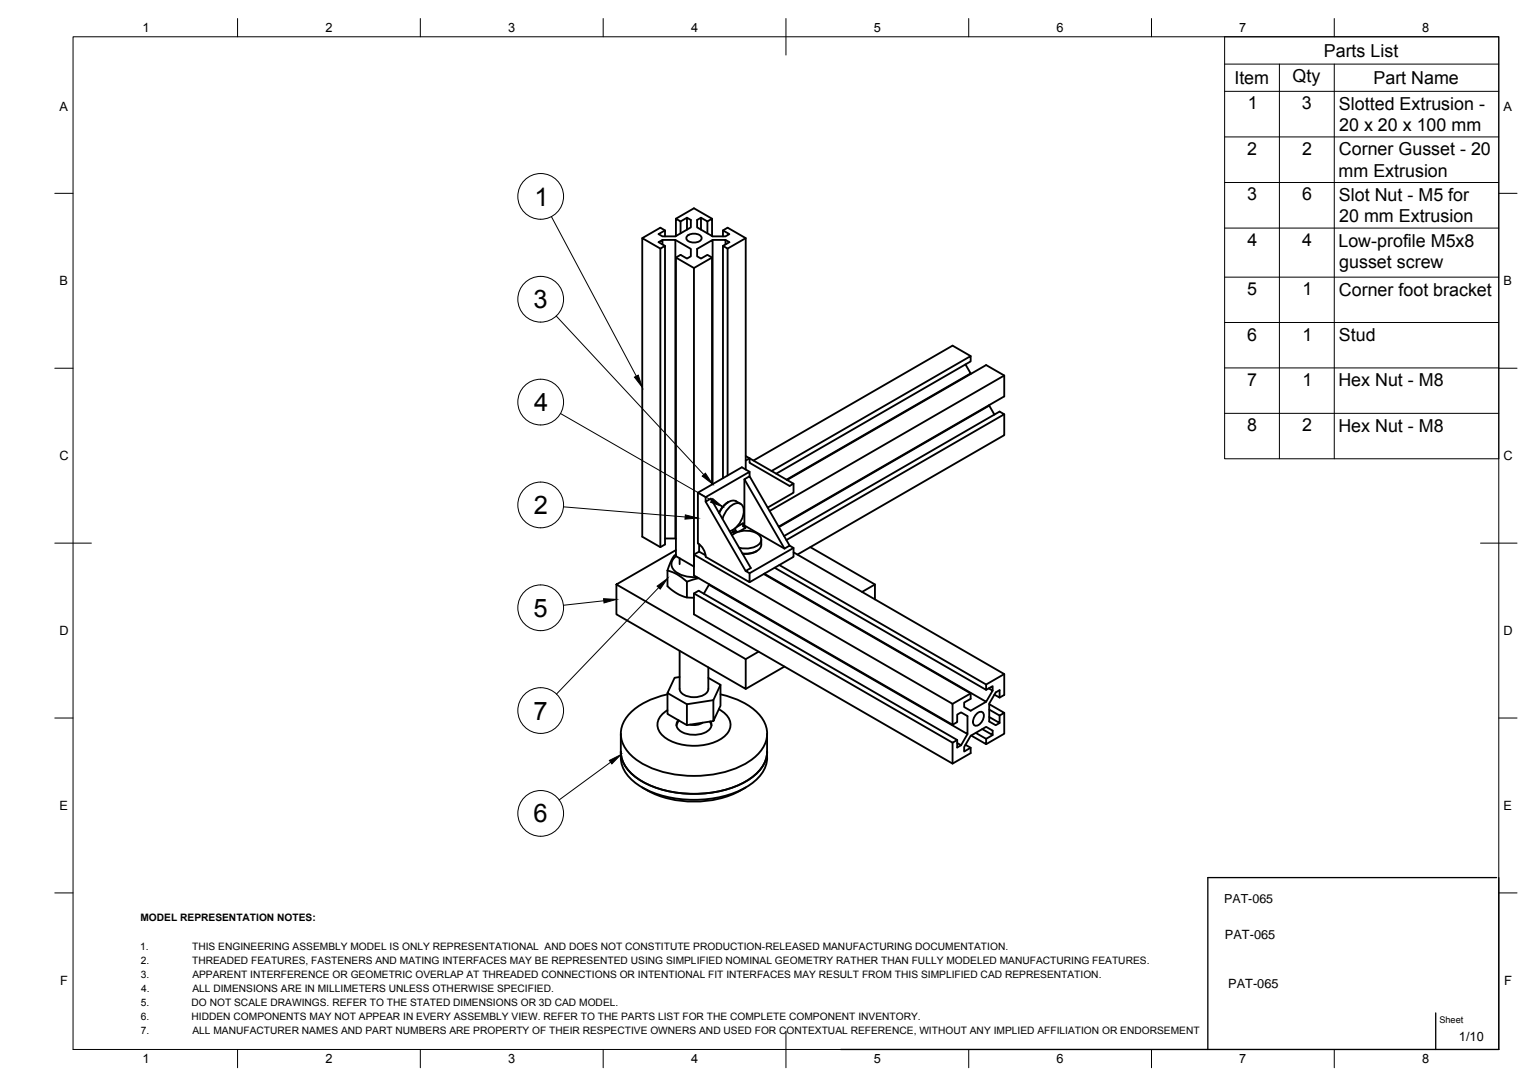
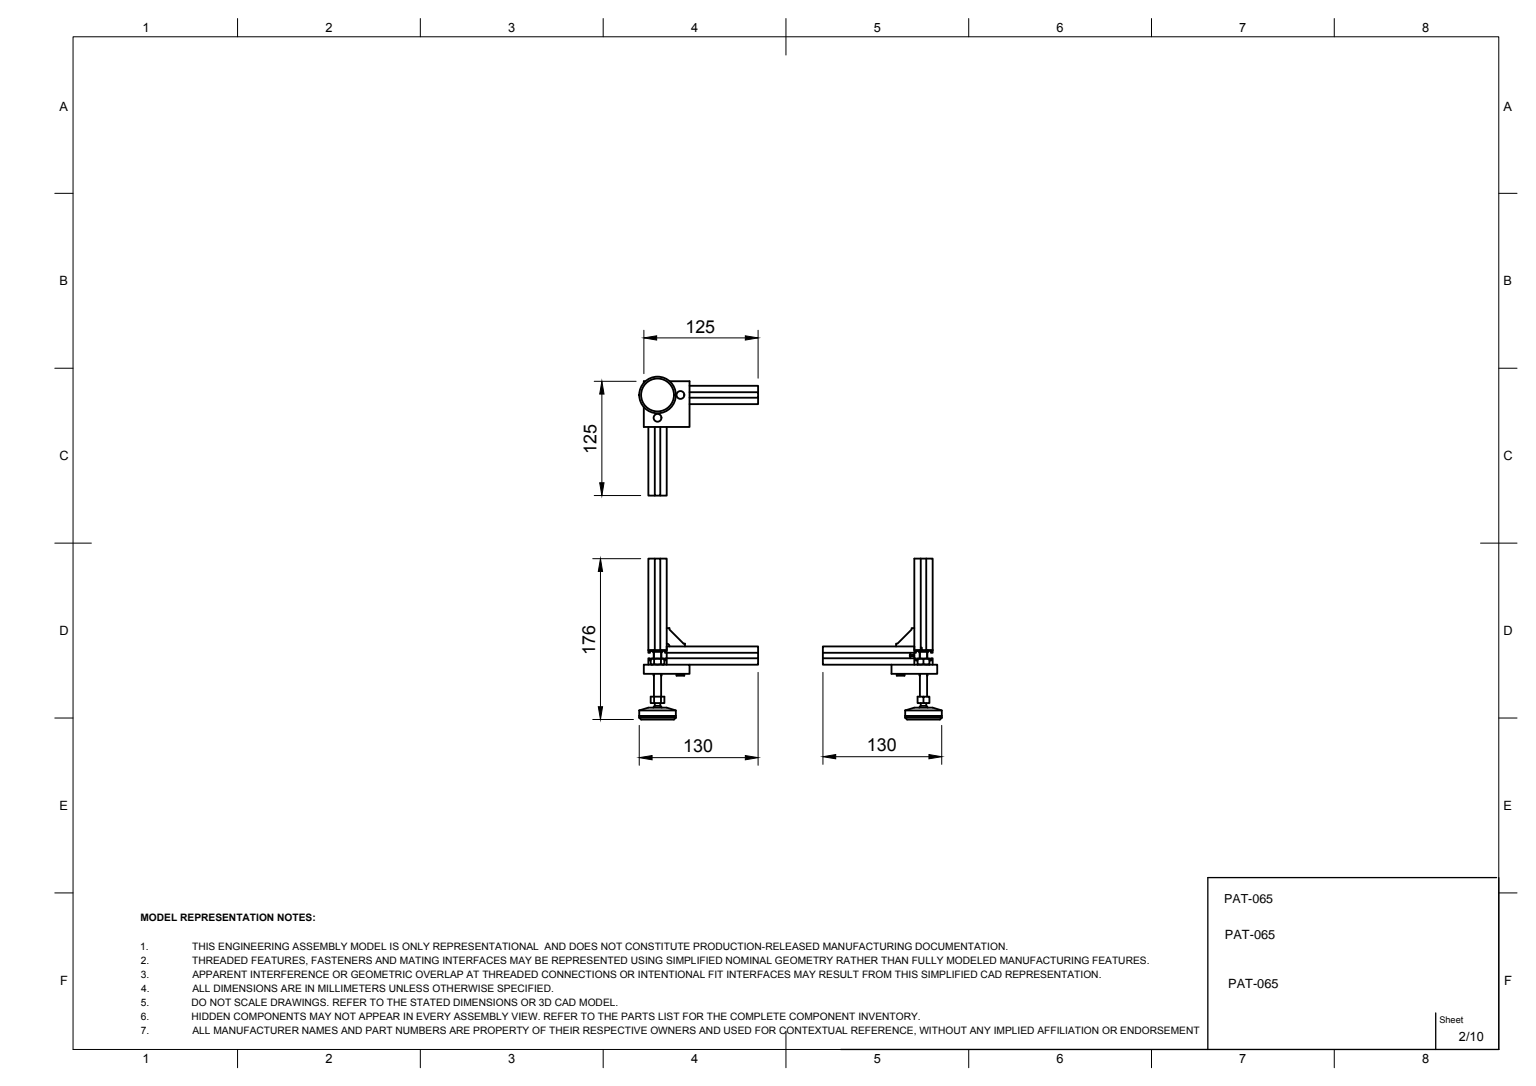
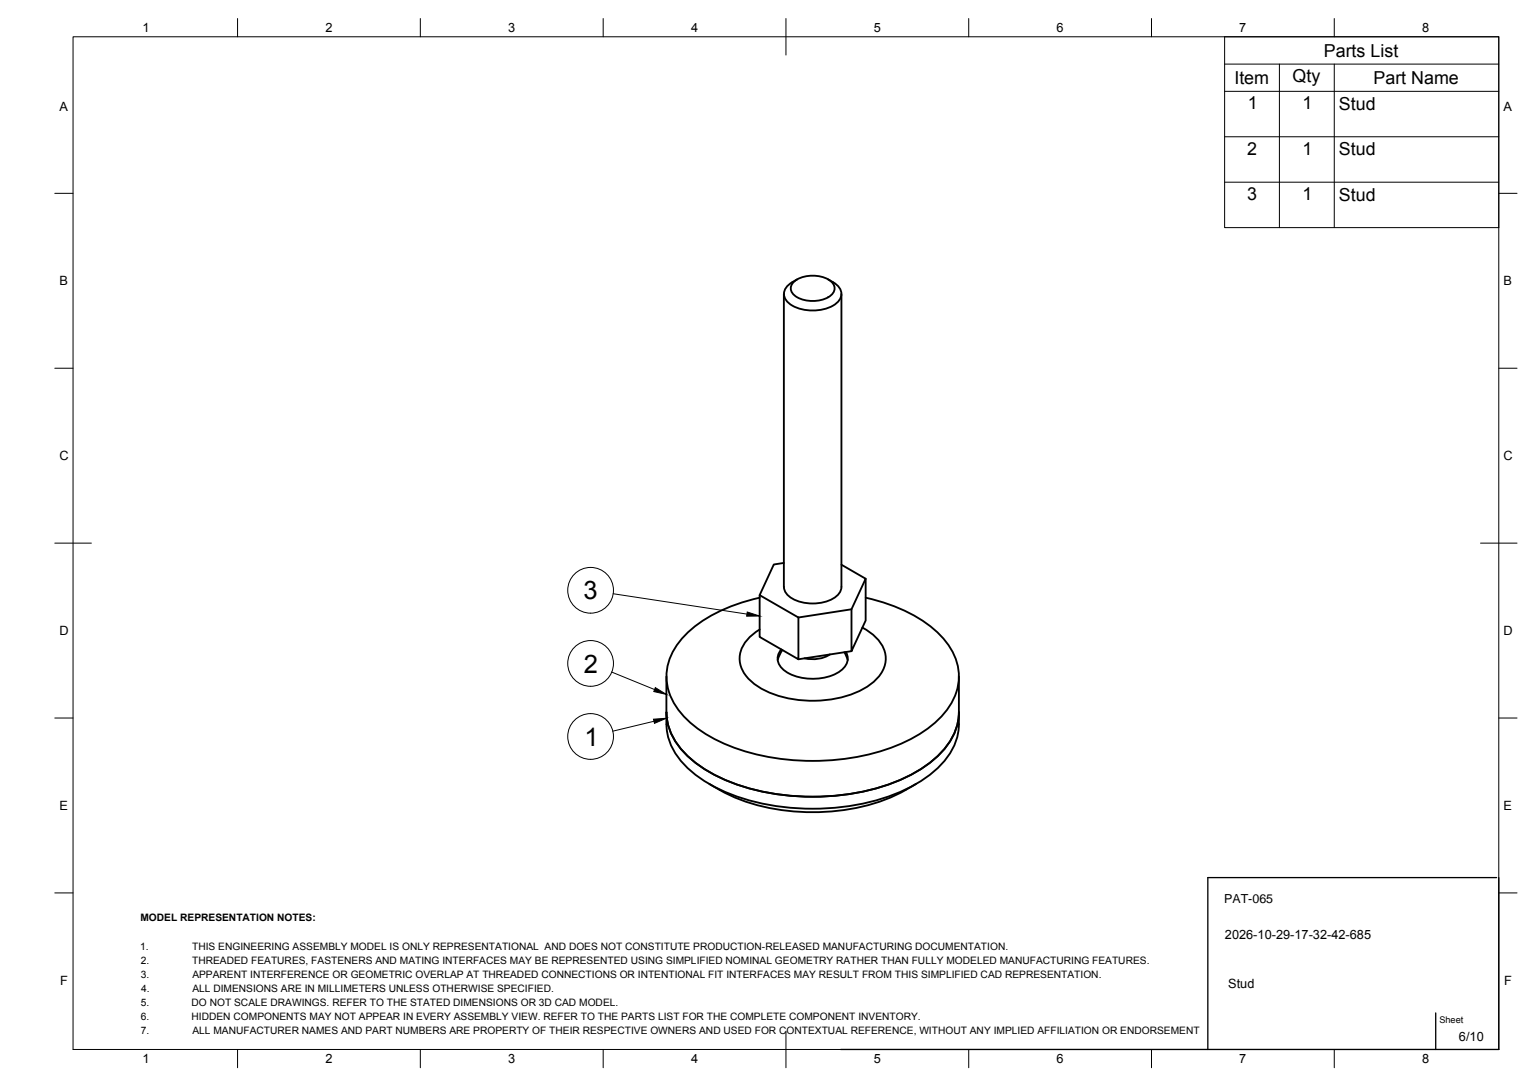
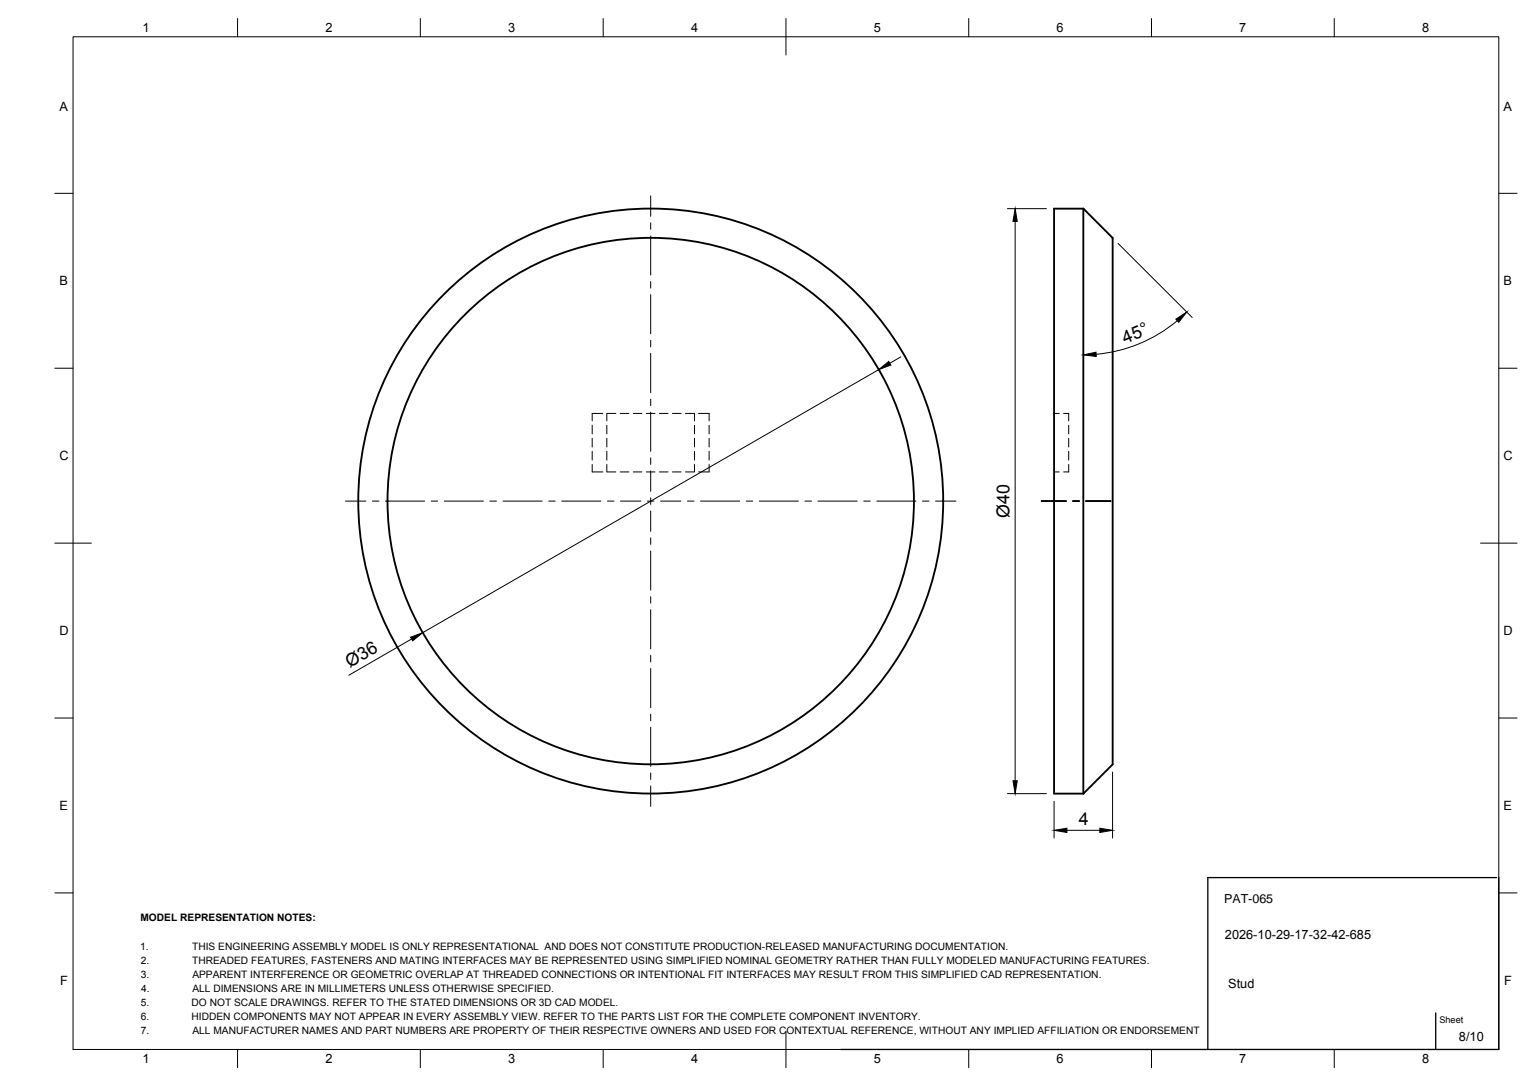
ISO-10303-21;
HEADER;
/* Generated by software containing ST-Developer
 * from STEP Tools, Inc. (www.steptools.com) 
 */

FILE_DESCRIPTION(
/* description */ ('PAT-065'),
/* implementation_level */ '2;1');

FILE_NAME(
/* name */ 'PAT-065',
/* time_stamp */ '2026-10-28T22:09:22-07:00',
/* author */ (''),
/* organization */ (''),
/* preprocessor_version */ 'ST-DEVELOPER v20.2',
/* originating_system */ 'Autodesk Translation Framework v15.17.0.0',
/* authorisation */ '');

FILE_SCHEMA (('AUTOMOTIVE_DESIGN { 1 0 10303 214 3 1 1 }'));
ENDSEC;

DATA;
#10=MECHANICAL_DESIGN_GEOMETRIC_PRESENTATION_REPRESENTATION('',(#158,#159,
#160,#161,#162,#163,#164,#165,#166,#167),#5502);
#11=(
BOUNDED_CURVE()
B_SPLINE_CURVE(2,(#5238,#5239,#5240),.UNSPECIFIED.,.F.,.F.)
B_SPLINE_CURVE_WITH_KNOTS((3,3),(0.14973948338295,0.97160236658079),
 .UNSPECIFIED.)
CURVE()
GEOMETRIC_REPRESENTATION_ITEM()
RATIONAL_B_SPLINE_CURVE((1.07140024848292,1.23714644374248,1.07140024848292))
REPRESENTATION_ITEM('')
);
#12=(
BOUNDED_CURVE()
B_SPLINE_CURVE(2,(#5242,#5243,#5244),.UNSPECIFIED.,.F.,.F.)
B_SPLINE_CURVE_WITH_KNOTS((3,3),(0.14973948338295,0.971602366580789),
 .UNSPECIFIED.)
CURVE()
GEOMETRIC_REPRESENTATION_ITEM()
RATIONAL_B_SPLINE_CURVE((1.07140024848292,1.23714644374248,1.07140024848292))
REPRESENTATION_ITEM('')
);
#13=(
BOUNDED_CURVE()
B_SPLINE_CURVE(2,(#5249,#5250,#5251),.UNSPECIFIED.,.F.,.F.)
B_SPLINE_CURVE_WITH_KNOTS((3,3),(0.14973948338295,0.97160236658079),
 .UNSPECIFIED.)
CURVE()
GEOMETRIC_REPRESENTATION_ITEM()
RATIONAL_B_SPLINE_CURVE((1.07140024848292,1.23714644374248,1.07140024848292))
REPRESENTATION_ITEM('')
);
#14=(
BOUNDED_CURVE()
B_SPLINE_CURVE(2,(#5253,#5254,#5255),.UNSPECIFIED.,.F.,.F.)
B_SPLINE_CURVE_WITH_KNOTS((3,3),(0.14973948338295,0.97160236658079),
 .UNSPECIFIED.)
CURVE()
GEOMETRIC_REPRESENTATION_ITEM()
RATIONAL_B_SPLINE_CURVE((1.07140024848292,1.23714644374248,1.07140024848292))
REPRESENTATION_ITEM('')
);
#15=(
BOUNDED_CURVE()
B_SPLINE_CURVE(2,(#5257,#5258,#5259),.UNSPECIFIED.,.F.,.F.)
B_SPLINE_CURVE_WITH_KNOTS((3,3),(0.14973948338295,0.971602366580789),
 .UNSPECIFIED.)
CURVE()
GEOMETRIC_REPRESENTATION_ITEM()
RATIONAL_B_SPLINE_CURVE((1.07140024848292,1.23714644374248,1.07140024848292))
REPRESENTATION_ITEM('')
);
#16=(
BOUNDED_CURVE()
B_SPLINE_CURVE(2,(#5260,#5261,#5262),.UNSPECIFIED.,.F.,.F.)
B_SPLINE_CURVE_WITH_KNOTS((3,3),(0.14973948338295,0.97160236658079),
 .UNSPECIFIED.)
CURVE()
GEOMETRIC_REPRESENTATION_ITEM()
RATIONAL_B_SPLINE_CURVE((1.07140024848292,1.23714644374248,1.07140024848292))
REPRESENTATION_ITEM('')
);
#17=(
BOUNDED_CURVE()
B_SPLINE_CURVE(2,(#5269,#5270,#5271),.UNSPECIFIED.,.F.,.F.)
B_SPLINE_CURVE_WITH_KNOTS((3,3),(0.14973948338295,0.97160236658079),
 .UNSPECIFIED.)
CURVE()
GEOMETRIC_REPRESENTATION_ITEM()
RATIONAL_B_SPLINE_CURVE((1.07140024848292,1.23714644374248,1.07140024848292))
REPRESENTATION_ITEM('')
);
#18=(
BOUNDED_CURVE()
B_SPLINE_CURVE(2,(#5273,#5274,#5275),.UNSPECIFIED.,.F.,.F.)
B_SPLINE_CURVE_WITH_KNOTS((3,3),(0.14973948338295,0.97160236658079),
 .UNSPECIFIED.)
CURVE()
GEOMETRIC_REPRESENTATION_ITEM()
RATIONAL_B_SPLINE_CURVE((1.07140024848292,1.23714644374248,1.07140024848292))
REPRESENTATION_ITEM('')
);
#19=(
BOUNDED_CURVE()
B_SPLINE_CURVE(2,(#5277,#5278,#5279),.UNSPECIFIED.,.F.,.F.)
B_SPLINE_CURVE_WITH_KNOTS((3,3),(0.14973948338295,0.971602366580789),
 .UNSPECIFIED.)
CURVE()
GEOMETRIC_REPRESENTATION_ITEM()
RATIONAL_B_SPLINE_CURVE((1.07140024848292,1.23714644374248,1.07140024848292))
REPRESENTATION_ITEM('')
);
#20=(
BOUNDED_CURVE()
B_SPLINE_CURVE(2,(#5281,#5282,#5283),.UNSPECIFIED.,.F.,.F.)
B_SPLINE_CURVE_WITH_KNOTS((3,3),(0.14973948338295,0.97160236658079),
 .UNSPECIFIED.)
CURVE()
GEOMETRIC_REPRESENTATION_ITEM()
RATIONAL_B_SPLINE_CURVE((1.07140024848292,1.23714644374248,1.07140024848292))
REPRESENTATION_ITEM('')
);
#21=(
BOUNDED_CURVE()
B_SPLINE_CURVE(2,(#5285,#5286,#5287),.UNSPECIFIED.,.F.,.F.)
B_SPLINE_CURVE_WITH_KNOTS((3,3),(0.14973948338295,0.97160236658079),
 .UNSPECIFIED.)
CURVE()
GEOMETRIC_REPRESENTATION_ITEM()
RATIONAL_B_SPLINE_CURVE((1.07140024848292,1.23714644374248,1.07140024848292))
REPRESENTATION_ITEM('')
);
#22=(
BOUNDED_CURVE()
B_SPLINE_CURVE(2,(#5288,#5289,#5290),.UNSPECIFIED.,.F.,.F.)
B_SPLINE_CURVE_WITH_KNOTS((3,3),(0.14973948338295,0.971602366580789),
 .UNSPECIFIED.)
CURVE()
GEOMETRIC_REPRESENTATION_ITEM()
RATIONAL_B_SPLINE_CURVE((1.07140024848292,1.23714644374248,1.07140024848292))
REPRESENTATION_ITEM('')
);
#23=ITEM_DEFINED_TRANSFORMATION($,$,#3464,#3521);
#24=ITEM_DEFINED_TRANSFORMATION($,$,#3481,#3522);
#25=ITEM_DEFINED_TRANSFORMATION($,$,#3496,#3523);
#26=ITEM_DEFINED_TRANSFORMATION($,$,#3328,#3598);
#27=ITEM_DEFINED_TRANSFORMATION($,$,#3344,#3599);
#28=ITEM_DEFINED_TRANSFORMATION($,$,#3344,#3600);
#29=ITEM_DEFINED_TRANSFORMATION($,$,#3344,#3601);
#30=ITEM_DEFINED_TRANSFORMATION($,$,#3411,#3602);
#31=ITEM_DEFINED_TRANSFORMATION($,$,#3411,#3603);
#32=ITEM_DEFINED_TRANSFORMATION($,$,#3548,#3604);
#33=ITEM_DEFINED_TRANSFORMATION($,$,#3442,#3605);
#34=ITEM_DEFINED_TRANSFORMATION($,$,#3548,#3606);
#35=ITEM_DEFINED_TRANSFORMATION($,$,#3442,#3607);
#36=ITEM_DEFINED_TRANSFORMATION($,$,#3548,#3608);
#37=ITEM_DEFINED_TRANSFORMATION($,$,#3442,#3609);
#38=ITEM_DEFINED_TRANSFORMATION($,$,#3548,#3610);
#39=ITEM_DEFINED_TRANSFORMATION($,$,#3442,#3611);
#40=ITEM_DEFINED_TRANSFORMATION($,$,#3463,#3612);
#41=ITEM_DEFINED_TRANSFORMATION($,$,#3524,#3613);
#42=ITEM_DEFINED_TRANSFORMATION($,$,#3548,#3614);
#43=ITEM_DEFINED_TRANSFORMATION($,$,#3577,#3615);
#44=ITEM_DEFINED_TRANSFORMATION($,$,#3548,#3616);
#45=ITEM_DEFINED_TRANSFORMATION($,$,#3577,#3617);
#46=(
REPRESENTATION_RELATIONSHIP($,$,#5560,#5559)
REPRESENTATION_RELATIONSHIP_WITH_TRANSFORMATION(#23)
SHAPE_REPRESENTATION_RELATIONSHIP()
);
#47=(
REPRESENTATION_RELATIONSHIP($,$,#5561,#5559)
REPRESENTATION_RELATIONSHIP_WITH_TRANSFORMATION(#24)
SHAPE_REPRESENTATION_RELATIONSHIP()
);
#48=(
REPRESENTATION_RELATIONSHIP($,$,#5562,#5559)
REPRESENTATION_RELATIONSHIP_WITH_TRANSFORMATION(#25)
SHAPE_REPRESENTATION_RELATIONSHIP()
);
#49=(
REPRESENTATION_RELATIONSHIP($,$,#5555,#5554)
REPRESENTATION_RELATIONSHIP_WITH_TRANSFORMATION(#26)
SHAPE_REPRESENTATION_RELATIONSHIP()
);
#50=(
REPRESENTATION_RELATIONSHIP($,$,#5556,#5554)
REPRESENTATION_RELATIONSHIP_WITH_TRANSFORMATION(#27)
SHAPE_REPRESENTATION_RELATIONSHIP()
);
#51=(
REPRESENTATION_RELATIONSHIP($,$,#5556,#5554)
REPRESENTATION_RELATIONSHIP_WITH_TRANSFORMATION(#28)
SHAPE_REPRESENTATION_RELATIONSHIP()
);
#52=(
REPRESENTATION_RELATIONSHIP($,$,#5556,#5554)
REPRESENTATION_RELATIONSHIP_WITH_TRANSFORMATION(#29)
SHAPE_REPRESENTATION_RELATIONSHIP()
);
#53=(
REPRESENTATION_RELATIONSHIP($,$,#5557,#5554)
REPRESENTATION_RELATIONSHIP_WITH_TRANSFORMATION(#30)
SHAPE_REPRESENTATION_RELATIONSHIP()
);
#54=(
REPRESENTATION_RELATIONSHIP($,$,#5557,#5554)
REPRESENTATION_RELATIONSHIP_WITH_TRANSFORMATION(#31)
SHAPE_REPRESENTATION_RELATIONSHIP()
);
#55=(
REPRESENTATION_RELATIONSHIP($,$,#5564,#5554)
REPRESENTATION_RELATIONSHIP_WITH_TRANSFORMATION(#32)
SHAPE_REPRESENTATION_RELATIONSHIP()
);
#56=(
REPRESENTATION_RELATIONSHIP($,$,#5558,#5554)
REPRESENTATION_RELATIONSHIP_WITH_TRANSFORMATION(#33)
SHAPE_REPRESENTATION_RELATIONSHIP()
);
#57=(
REPRESENTATION_RELATIONSHIP($,$,#5564,#5554)
REPRESENTATION_RELATIONSHIP_WITH_TRANSFORMATION(#34)
SHAPE_REPRESENTATION_RELATIONSHIP()
);
#58=(
REPRESENTATION_RELATIONSHIP($,$,#5558,#5554)
REPRESENTATION_RELATIONSHIP_WITH_TRANSFORMATION(#35)
SHAPE_REPRESENTATION_RELATIONSHIP()
);
#59=(
REPRESENTATION_RELATIONSHIP($,$,#5564,#5554)
REPRESENTATION_RELATIONSHIP_WITH_TRANSFORMATION(#36)
SHAPE_REPRESENTATION_RELATIONSHIP()
);
#60=(
REPRESENTATION_RELATIONSHIP($,$,#5558,#5554)
REPRESENTATION_RELATIONSHIP_WITH_TRANSFORMATION(#37)
SHAPE_REPRESENTATION_RELATIONSHIP()
);
#61=(
REPRESENTATION_RELATIONSHIP($,$,#5564,#5554)
REPRESENTATION_RELATIONSHIP_WITH_TRANSFORMATION(#38)
SHAPE_REPRESENTATION_RELATIONSHIP()
);
#62=(
REPRESENTATION_RELATIONSHIP($,$,#5558,#5554)
REPRESENTATION_RELATIONSHIP_WITH_TRANSFORMATION(#39)
SHAPE_REPRESENTATION_RELATIONSHIP()
);
#63=(
REPRESENTATION_RELATIONSHIP($,$,#5559,#5554)
REPRESENTATION_RELATIONSHIP_WITH_TRANSFORMATION(#40)
SHAPE_REPRESENTATION_RELATIONSHIP()
);
#64=(
REPRESENTATION_RELATIONSHIP($,$,#5563,#5554)
REPRESENTATION_RELATIONSHIP_WITH_TRANSFORMATION(#41)
SHAPE_REPRESENTATION_RELATIONSHIP()
);
#65=(
REPRESENTATION_RELATIONSHIP($,$,#5564,#5554)
REPRESENTATION_RELATIONSHIP_WITH_TRANSFORMATION(#42)
SHAPE_REPRESENTATION_RELATIONSHIP()
);
#66=(
REPRESENTATION_RELATIONSHIP($,$,#5565,#5554)
REPRESENTATION_RELATIONSHIP_WITH_TRANSFORMATION(#43)
SHAPE_REPRESENTATION_RELATIONSHIP()
);
#67=(
REPRESENTATION_RELATIONSHIP($,$,#5564,#5554)
REPRESENTATION_RELATIONSHIP_WITH_TRANSFORMATION(#44)
SHAPE_REPRESENTATION_RELATIONSHIP()
);
#68=(
REPRESENTATION_RELATIONSHIP($,$,#5565,#5554)
REPRESENTATION_RELATIONSHIP_WITH_TRANSFORMATION(#45)
SHAPE_REPRESENTATION_RELATIONSHIP()
);
#69=CONTEXT_DEPENDENT_SHAPE_REPRESENTATION(#46,#5528);
#70=CONTEXT_DEPENDENT_SHAPE_REPRESENTATION(#47,#5529);
#71=CONTEXT_DEPENDENT_SHAPE_REPRESENTATION(#48,#5530);
#72=CONTEXT_DEPENDENT_SHAPE_REPRESENTATION(#49,#5534);
#73=CONTEXT_DEPENDENT_SHAPE_REPRESENTATION(#50,#5535);
#74=CONTEXT_DEPENDENT_SHAPE_REPRESENTATION(#51,#5536);
#75=CONTEXT_DEPENDENT_SHAPE_REPRESENTATION(#52,#5537);
#76=CONTEXT_DEPENDENT_SHAPE_REPRESENTATION(#53,#5538);
#77=CONTEXT_DEPENDENT_SHAPE_REPRESENTATION(#54,#5539);
#78=CONTEXT_DEPENDENT_SHAPE_REPRESENTATION(#55,#5540);
#79=CONTEXT_DEPENDENT_SHAPE_REPRESENTATION(#56,#5541);
#80=CONTEXT_DEPENDENT_SHAPE_REPRESENTATION(#57,#5542);
#81=CONTEXT_DEPENDENT_SHAPE_REPRESENTATION(#58,#5543);
#82=CONTEXT_DEPENDENT_SHAPE_REPRESENTATION(#59,#5544);
#83=CONTEXT_DEPENDENT_SHAPE_REPRESENTATION(#60,#5545);
#84=CONTEXT_DEPENDENT_SHAPE_REPRESENTATION(#61,#5546);
#85=CONTEXT_DEPENDENT_SHAPE_REPRESENTATION(#62,#5547);
#86=CONTEXT_DEPENDENT_SHAPE_REPRESENTATION(#63,#5548);
#87=CONTEXT_DEPENDENT_SHAPE_REPRESENTATION(#64,#5549);
#88=CONTEXT_DEPENDENT_SHAPE_REPRESENTATION(#65,#5550);
#89=CONTEXT_DEPENDENT_SHAPE_REPRESENTATION(#66,#5551);
#90=CONTEXT_DEPENDENT_SHAPE_REPRESENTATION(#67,#5552);
#91=CONTEXT_DEPENDENT_SHAPE_REPRESENTATION(#68,#5553);
#92=NEXT_ASSEMBLY_USAGE_OCCURRENCE('Rubber base:1','Rubber base:1',
'Rubber base:1',#5572,#5573,'Rubber base:1');
#93=NEXT_ASSEMBLY_USAGE_OCCURRENCE('Steel pad:1','Steel pad:1',
'Steel pad:1',#5572,#5574,'Steel pad:1');
#94=NEXT_ASSEMBLY_USAGE_OCCURRENCE('Stud:1','Stud:1','Stud:1',#5572,#5575,
'Stud:1');
#95=NEXT_ASSEMBLY_USAGE_OCCURRENCE('Corner foot bracket:1',
'Corner foot bracket:1','Corner foot bracket:1',#5567,#5568,
'Corner foot bracket:1');
#96=NEXT_ASSEMBLY_USAGE_OCCURRENCE(
'Slotted Extrusion - 20 x 20 x 100 mm:1',
'Slotted Extrusion - 20 x 20 x 100 mm:1',
'Slotted Extrusion - 20 x 20 x 100 mm:1',#5567,#5569,
'Slotted Extrusion - 20 x 20 x 100 mm:1');
#97=NEXT_ASSEMBLY_USAGE_OCCURRENCE(
'Slotted Extrusion - 20 x 20 x 100 mm:2',
'Slotted Extrusion - 20 x 20 x 100 mm:2',
'Slotted Extrusion - 20 x 20 x 100 mm:2',#5567,#5569,
'Slotted Extrusion - 20 x 20 x 100 mm:2');
#98=NEXT_ASSEMBLY_USAGE_OCCURRENCE(
'Slotted Extrusion - 20 x 20 x 100 mm:3',
'Slotted Extrusion - 20 x 20 x 100 mm:3',
'Slotted Extrusion - 20 x 20 x 100 mm:3',#5567,#5569,
'Slotted Extrusion - 20 x 20 x 100 mm:3');
#99=NEXT_ASSEMBLY_USAGE_OCCURRENCE('Corner Gusset - 20 mm Extrusion:1',
'Corner Gusset - 20 mm Extrusion:1','Corner Gusset - 20 mm Extrusion:1',
#5567,#5570,'Corner Gusset - 20 mm Extrusion:1');
#100=NEXT_ASSEMBLY_USAGE_OCCURRENCE('Corner Gusset - 20 mm Extrusion:2',
'Corner Gusset - 20 mm Extrusion:2','Corner Gusset - 20 mm Extrusion:2',
#5567,#5570,'Corner Gusset - 20 mm Extrusion:2');
#101=NEXT_ASSEMBLY_USAGE_OCCURRENCE(
'Slot Nut - M5 for 20 mm Extrusion:1',
'Slot Nut - M5 for 20 mm Extrusion:1',
'Slot Nut - M5 for 20 mm Extrusion:1',#5567,#5577,
'Slot Nut - M5 for 20 mm Extrusion:1');
#102=NEXT_ASSEMBLY_USAGE_OCCURRENCE('Low-profile M5x8 gusset screw:1',
'Low-profile M5x8 gusset screw:1','Low-profile M5x8 gusset screw:1',#5567,
#5571,'Low-profile M5x8 gusset screw:1');
#103=NEXT_ASSEMBLY_USAGE_OCCURRENCE(
'Slot Nut - M5 for 20 mm Extrusion:2',
'Slot Nut - M5 for 20 mm Extrusion:2',
'Slot Nut - M5 for 20 mm Extrusion:2',#5567,#5577,
'Slot Nut - M5 for 20 mm Extrusion:2');
#104=NEXT_ASSEMBLY_USAGE_OCCURRENCE('Low-profile M5x8 gusset screw:2',
'Low-profile M5x8 gusset screw:2','Low-profile M5x8 gusset screw:2',#5567,
#5571,'Low-profile M5x8 gusset screw:2');
#105=NEXT_ASSEMBLY_USAGE_OCCURRENCE(
'Slot Nut - M5 for 20 mm Extrusion:3',
'Slot Nut - M5 for 20 mm Extrusion:3',
'Slot Nut - M5 for 20 mm Extrusion:3',#5567,#5577,
'Slot Nut - M5 for 20 mm Extrusion:3');
#106=NEXT_ASSEMBLY_USAGE_OCCURRENCE('Low-profile M5x8 gusset screw:3',
'Low-profile M5x8 gusset screw:3','Low-profile M5x8 gusset screw:3',#5567,
#5571,'Low-profile M5x8 gusset screw:3');
#107=NEXT_ASSEMBLY_USAGE_OCCURRENCE(
'Slot Nut - M5 for 20 mm Extrusion:4',
'Slot Nut - M5 for 20 mm Extrusion:4',
'Slot Nut - M5 for 20 mm Extrusion:4',#5567,#5577,
'Slot Nut - M5 for 20 mm Extrusion:4');
#108=NEXT_ASSEMBLY_USAGE_OCCURRENCE('Low-profile M5x8 gusset screw:4',
'Low-profile M5x8 gusset screw:4','Low-profile M5x8 gusset screw:4',#5567,
#5571,'Low-profile M5x8 gusset screw:4');
#109=NEXT_ASSEMBLY_USAGE_OCCURRENCE(
'Levelling Foot - 40 mm Pad, M8 Stud:1',
'Levelling Foot - 40 mm Pad, M8 Stud:1',
'Levelling Foot - 40 mm Pad, M8 Stud:1',#5567,#5572,
'Levelling Foot - 40 mm Pad, M8 Stud:1');
#110=NEXT_ASSEMBLY_USAGE_OCCURRENCE('Hex Nut - M8:1','Hex Nut - M8:1',
'Hex Nut - M8:1',#5567,#5576,'Hex Nut - M8:1');
#111=NEXT_ASSEMBLY_USAGE_OCCURRENCE(
'Slot Nut - M5 for 20 mm Extrusion:5',
'Slot Nut - M5 for 20 mm Extrusion:5',
'Slot Nut - M5 for 20 mm Extrusion:5',#5567,#5577,
'Slot Nut - M5 for 20 mm Extrusion:5');
#112=NEXT_ASSEMBLY_USAGE_OCCURRENCE('M5x14 Cap Screw:1',
'M5x14 Cap Screw:1','M5x14 Cap Screw:1',#5567,#5578,'M5x14 Cap Screw:1');
#113=NEXT_ASSEMBLY_USAGE_OCCURRENCE(
'Slot Nut - M5 for 20 mm Extrusion:6',
'Slot Nut - M5 for 20 mm Extrusion:6',
'Slot Nut - M5 for 20 mm Extrusion:6',#5567,#5577,
'Slot Nut - M5 for 20 mm Extrusion:6');
#114=NEXT_ASSEMBLY_USAGE_OCCURRENCE('M5x14 Cap Screw:2',
'M5x14 Cap Screw:2','M5x14 Cap Screw:2',#5567,#5578,'M5x14 Cap Screw:2');
#115=ORIENTED_CLOSED_SHELL('',*,#3212,.F.);
#116=BREP_WITH_VOIDS('Body1',#3211,(#115));
#117=SPHERICAL_SURFACE('',#3486,0.52);
#118=SPHERICAL_SURFACE('',#3514,0.5);
#119=CONICAL_SURFACE('',#3449,0.41,0.785398163397448);
#120=CONICAL_SURFACE('',#3453,0.26,0.463647609000806);
#121=CONICAL_SURFACE('',#3465,1.9,0.785398163397448);
#122=CONICAL_SURFACE('',#3493,1.5,1.27933953231703);
#123=CONICAL_SURFACE('',#3511,0.35,0.78539816339745);
#124=CONICAL_SURFACE('',#3534,0.734027674973257,1.0471975511966);
#125=CONICAL_SURFACE('',#3536,0.734027674973257,1.0471975511966);
#126=CONICAL_SURFACE('',#3584,0.41,0.785398163397448);
#127=CONICAL_SURFACE('',#3588,0.26,0.463647609000806);
#128=B_SPLINE_CURVE_WITH_KNOTS('',3,(#4608,#4609,#4610,#4611,#4612,#4613),
 .UNSPECIFIED.,.F.,.F.,(4,2,4),(0.899292285450093,0.96236755734344,1.02544282923679),
 .UNSPECIFIED.);
#129=ELLIPSE('',#3350,0.707106781186548,0.5);
#130=ELLIPSE('',#3352,0.707106781186547,0.5);
#131=ELLIPSE('',#3354,0.707106781186548,0.5);
#132=ELLIPSE('',#3355,0.707106781186548,0.5);
#133=ELLIPSE('',#3550,0.707106781186548,0.5);
#134=ELLIPSE('',#3555,0.707106781186548,0.5);
#135=ELLIPSE('',#3562,0.299389011154384,0.2117);
#136=ELLIPSE('',#3564,0.299389011154384,0.2117);
#137=ELLIPSE('',#3566,0.299389011154384,0.2117);
#138=SHAPE_REPRESENTATION_RELATIONSHIP('SRR','None',#5555,#148);
#139=SHAPE_REPRESENTATION_RELATIONSHIP('SRR','None',#5556,#149);
#140=SHAPE_REPRESENTATION_RELATIONSHIP('SRR','None',#5557,#150);
#141=SHAPE_REPRESENTATION_RELATIONSHIP('SRR','None',#5558,#151);
#142=SHAPE_REPRESENTATION_RELATIONSHIP('SRR','None',#5560,#152);
#143=SHAPE_REPRESENTATION_RELATIONSHIP('SRR','None',#5561,#153);
#144=SHAPE_REPRESENTATION_RELATIONSHIP('SRR','None',#5562,#154);
#145=SHAPE_REPRESENTATION_RELATIONSHIP('SRR','None',#5563,#155);
#146=SHAPE_REPRESENTATION_RELATIONSHIP('SRR','None',#5564,#156);
#147=SHAPE_REPRESENTATION_RELATIONSHIP('SRR','None',#5565,#157);
#148=ADVANCED_BREP_SHAPE_REPRESENTATION('',(#168),#5491);
#149=ADVANCED_BREP_SHAPE_REPRESENTATION('',(#169),#5492);
#150=ADVANCED_BREP_SHAPE_REPRESENTATION('',(#170),#5493);
#151=ADVANCED_BREP_SHAPE_REPRESENTATION('',(#171),#5494);
#152=ADVANCED_BREP_SHAPE_REPRESENTATION('',(#172),#5496);
#153=ADVANCED_BREP_SHAPE_REPRESENTATION('',(#173),#5497);
#154=ADVANCED_BREP_SHAPE_REPRESENTATION('',(#116),#5498);
#155=ADVANCED_BREP_SHAPE_REPRESENTATION('',(#174),#5499);
#156=ADVANCED_BREP_SHAPE_REPRESENTATION('',(#175),#5500);
#157=ADVANCED_BREP_SHAPE_REPRESENTATION('',(#176),#5501);
#158=STYLED_ITEM('',(#5673),#168);
#159=STYLED_ITEM('',(#5708),#169);
#160=STYLED_ITEM('',(#5708),#170);
#161=STYLED_ITEM('',(#5701),#171);
#162=STYLED_ITEM('',(#5701),#172);
#163=STYLED_ITEM('',(#5680),#173);
#164=STYLED_ITEM('',(#5701),#116);
#165=STYLED_ITEM('',(#5701),#174);
#166=STYLED_ITEM('',(#5701),#175);
#167=STYLED_ITEM('',(#5701),#176);
#168=MANIFOLD_SOLID_BREP('Body1',#3205);
#169=MANIFOLD_SOLID_BREP('Body1',#3206);
#170=MANIFOLD_SOLID_BREP('Body1',#3207);
#171=MANIFOLD_SOLID_BREP('Body1',#3208);
#172=MANIFOLD_SOLID_BREP('Body1',#3209);
#173=MANIFOLD_SOLID_BREP('Body1',#3210);
#174=MANIFOLD_SOLID_BREP('Body1',#3213);
#175=MANIFOLD_SOLID_BREP('Body1',#3214);
#176=MANIFOLD_SOLID_BREP('Body1',#3215);
#177=FACE_BOUND('',#519,.T.);
#178=FACE_BOUND('',#520,.T.);
#179=FACE_BOUND('',#521,.T.);
#180=FACE_BOUND('',#523,.T.);
#181=FACE_BOUND('',#524,.T.);
#182=FACE_BOUND('',#525,.T.);
#183=FACE_BOUND('',#579,.T.);
#184=FACE_BOUND('',#586,.T.);
#185=FACE_BOUND('',#588,.T.);
#186=FACE_BOUND('',#596,.T.);
#187=FACE_BOUND('',#601,.T.);
#188=FACE_BOUND('',#607,.T.);
#189=FACE_BOUND('',#611,.T.);
#190=FACE_BOUND('',#630,.T.);
#191=FACE_BOUND('',#634,.T.);
#192=FACE_BOUND('',#639,.T.);
#193=FACE_BOUND('',#641,.T.);
#194=FACE_BOUND('',#650,.T.);
#195=FACE_BOUND('',#660,.T.);
#196=FACE_BOUND('',#662,.T.);
#197=FACE_BOUND('',#674,.T.);
#198=FACE_BOUND('',#676,.T.);
#199=FACE_BOUND('',#695,.T.);
#200=FACE_BOUND('',#699,.T.);
#201=PLANE('',#3338);
#202=PLANE('',#3339);
#203=PLANE('',#3340);
#204=PLANE('',#3341);
#205=PLANE('',#3342);
#206=PLANE('',#3343);
#207=PLANE('',#3345);
#208=PLANE('',#3347);
#209=PLANE('',#3357);
#210=PLANE('',#3358);
#211=PLANE('',#3359);
#212=PLANE('',#3360);
#213=PLANE('',#3361);
#214=PLANE('',#3362);
#215=PLANE('',#3363);
#216=PLANE('',#3364);
#217=PLANE('',#3367);
#218=PLANE('',#3368);
#219=PLANE('',#3369);
#220=PLANE('',#3370);
#221=PLANE('',#3371);
#222=PLANE('',#3372);
#223=PLANE('',#3373);
#224=PLANE('',#3374);
#225=PLANE('',#3375);
#226=PLANE('',#3376);
#227=PLANE('',#3377);
#228=PLANE('',#3378);
#229=PLANE('',#3379);
#230=PLANE('',#3380);
#231=PLANE('',#3381);
#232=PLANE('',#3382);
#233=PLANE('',#3383);
#234=PLANE('',#3384);
#235=PLANE('',#3385);
#236=PLANE('',#3386);
#237=PLANE('',#3387);
#238=PLANE('',#3388);
#239=PLANE('',#3389);
#240=PLANE('',#3390);
#241=PLANE('',#3391);
#242=PLANE('',#3392);
#243=PLANE('',#3393);
#244=PLANE('',#3394);
#245=PLANE('',#3395);
#246=PLANE('',#3396);
#247=PLANE('',#3397);
#248=PLANE('',#3398);
#249=PLANE('',#3401);
#250=PLANE('',#3402);
#251=PLANE('',#3403);
#252=PLANE('',#3404);
#253=PLANE('',#3405);
#254=PLANE('',#3406);
#255=PLANE('',#3407);
#256=PLANE('',#3408);
#257=PLANE('',#3409);
#258=PLANE('',#3410);
#259=PLANE('',#3412);
#260=PLANE('',#3419);
#261=PLANE('',#3420);
#262=PLANE('',#3422);
#263=PLANE('',#3424);
#264=PLANE('',#3432);
#265=PLANE('',#3433);
#266=PLANE('',#3434);
#267=PLANE('',#3435);
#268=PLANE('',#3436);
#269=PLANE('',#3437);
#270=PLANE('',#3438);
#271=PLANE('',#3439);
#272=PLANE('',#3440);
#273=PLANE('',#3441);
#274=PLANE('',#3443);
#275=PLANE('',#3445);
#276=PLANE('',#3451);
#277=PLANE('',#3456);
#278=PLANE('',#3457);
#279=PLANE('',#3458);
#280=PLANE('',#3459);
#281=PLANE('',#3460);
#282=PLANE('',#3461);
#283=PLANE('',#3462);
#284=PLANE('',#3468);
#285=PLANE('',#3471);
#286=PLANE('',#3472);
#287=PLANE('',#3477);
#288=PLANE('',#3480);
#289=PLANE('',#3482);
#290=PLANE('',#3484);
#291=PLANE('',#3489);
#292=PLANE('',#3495);
#293=PLANE('',#3497);
#294=PLANE('',#3499);
#295=PLANE('',#3500);
#296=PLANE('',#3501);
#297=PLANE('',#3502);
#298=PLANE('',#3503);
#299=PLANE('',#3504);
#300=PLANE('',#3508);
#301=PLANE('',#3513);
#302=PLANE('',#3519);
#303=PLANE('',#3520);
#304=PLANE('',#3528);
#305=PLANE('',#3530);
#306=PLANE('',#3538);
#307=PLANE('',#3539);
#308=PLANE('',#3540);
#309=PLANE('',#3543);
#310=PLANE('',#3544);
#311=PLANE('',#3545);
#312=PLANE('',#3546);
#313=PLANE('',#3547);
#314=PLANE('',#3557);
#315=PLANE('',#3558);
#316=PLANE('',#3559);
#317=PLANE('',#3560);
#318=PLANE('',#3561);
#319=PLANE('',#3563);
#320=PLANE('',#3565);
#321=PLANE('',#3571);
#322=PLANE('',#3572);
#323=PLANE('',#3573);
#324=PLANE('',#3574);
#325=PLANE('',#3575);
#326=PLANE('',#3576);
#327=PLANE('',#3578);
#328=PLANE('',#3580);
#329=PLANE('',#3586);
#330=PLANE('',#3591);
#331=PLANE('',#3592);
#332=PLANE('',#3593);
#333=PLANE('',#3594);
#334=PLANE('',#3595);
#335=PLANE('',#3596);
#336=PLANE('',#3597);
#337=FACE_OUTER_BOUND('',#511,.T.);
#338=FACE_OUTER_BOUND('',#512,.T.);
#339=FACE_OUTER_BOUND('',#513,.T.);
#340=FACE_OUTER_BOUND('',#514,.T.);
#341=FACE_OUTER_BOUND('',#515,.T.);
#342=FACE_OUTER_BOUND('',#516,.T.);
#343=FACE_OUTER_BOUND('',#517,.T.);
#344=FACE_OUTER_BOUND('',#518,.T.);
#345=FACE_OUTER_BOUND('',#522,.T.);
#346=FACE_OUTER_BOUND('',#526,.T.);
#347=FACE_OUTER_BOUND('',#527,.T.);
#348=FACE_OUTER_BOUND('',#528,.T.);
#349=FACE_OUTER_BOUND('',#529,.T.);
#350=FACE_OUTER_BOUND('',#530,.T.);
#351=FACE_OUTER_BOUND('',#531,.T.);
#352=FACE_OUTER_BOUND('',#532,.T.);
#353=FACE_OUTER_BOUND('',#533,.T.);
#354=FACE_OUTER_BOUND('',#534,.T.);
#355=FACE_OUTER_BOUND('',#535,.T.);
#356=FACE_OUTER_BOUND('',#536,.T.);
#357=FACE_OUTER_BOUND('',#537,.T.);
#358=FACE_OUTER_BOUND('',#538,.T.);
#359=FACE_OUTER_BOUND('',#539,.T.);
#360=FACE_OUTER_BOUND('',#540,.T.);
#361=FACE_OUTER_BOUND('',#541,.T.);
#362=FACE_OUTER_BOUND('',#542,.T.);
#363=FACE_OUTER_BOUND('',#543,.T.);
#364=FACE_OUTER_BOUND('',#544,.T.);
#365=FACE_OUTER_BOUND('',#545,.T.);
#366=FACE_OUTER_BOUND('',#546,.T.);
#367=FACE_OUTER_BOUND('',#547,.T.);
#368=FACE_OUTER_BOUND('',#548,.T.);
#369=FACE_OUTER_BOUND('',#549,.T.);
#370=FACE_OUTER_BOUND('',#550,.T.);
#371=FACE_OUTER_BOUND('',#551,.T.);
#372=FACE_OUTER_BOUND('',#552,.T.);
#373=FACE_OUTER_BOUND('',#553,.T.);
#374=FACE_OUTER_BOUND('',#554,.T.);
#375=FACE_OUTER_BOUND('',#555,.T.);
#376=FACE_OUTER_BOUND('',#556,.T.);
#377=FACE_OUTER_BOUND('',#557,.T.);
#378=FACE_OUTER_BOUND('',#558,.T.);
#379=FACE_OUTER_BOUND('',#559,.T.);
#380=FACE_OUTER_BOUND('',#560,.T.);
#381=FACE_OUTER_BOUND('',#561,.T.);
#382=FACE_OUTER_BOUND('',#562,.T.);
#383=FACE_OUTER_BOUND('',#563,.T.);
#384=FACE_OUTER_BOUND('',#564,.T.);
#385=FACE_OUTER_BOUND('',#565,.T.);
#386=FACE_OUTER_BOUND('',#566,.T.);
#387=FACE_OUTER_BOUND('',#567,.T.);
#388=FACE_OUTER_BOUND('',#568,.T.);
#389=FACE_OUTER_BOUND('',#569,.T.);
#390=FACE_OUTER_BOUND('',#570,.T.);
#391=FACE_OUTER_BOUND('',#571,.T.);
#392=FACE_OUTER_BOUND('',#572,.T.);
#393=FACE_OUTER_BOUND('',#573,.T.);
#394=FACE_OUTER_BOUND('',#574,.T.);
#395=FACE_OUTER_BOUND('',#575,.T.);
#396=FACE_OUTER_BOUND('',#576,.T.);
#397=FACE_OUTER_BOUND('',#577,.T.);
#398=FACE_OUTER_BOUND('',#578,.T.);
#399=FACE_OUTER_BOUND('',#580,.T.);
#400=FACE_OUTER_BOUND('',#581,.T.);
#401=FACE_OUTER_BOUND('',#582,.T.);
#402=FACE_OUTER_BOUND('',#583,.T.);
#403=FACE_OUTER_BOUND('',#584,.T.);
#404=FACE_OUTER_BOUND('',#585,.T.);
#405=FACE_OUTER_BOUND('',#587,.T.);
#406=FACE_OUTER_BOUND('',#589,.T.);
#407=FACE_OUTER_BOUND('',#590,.T.);
#408=FACE_OUTER_BOUND('',#591,.T.);
#409=FACE_OUTER_BOUND('',#592,.T.);
#410=FACE_OUTER_BOUND('',#593,.T.);
#411=FACE_OUTER_BOUND('',#594,.T.);
#412=FACE_OUTER_BOUND('',#595,.T.);
#413=FACE_OUTER_BOUND('',#597,.T.);
#414=FACE_OUTER_BOUND('',#598,.T.);
#415=FACE_OUTER_BOUND('',#599,.T.);
#416=FACE_OUTER_BOUND('',#600,.T.);
#417=FACE_OUTER_BOUND('',#602,.T.);
#418=FACE_OUTER_BOUND('',#603,.T.);
#419=FACE_OUTER_BOUND('',#604,.T.);
#420=FACE_OUTER_BOUND('',#605,.T.);
#421=FACE_OUTER_BOUND('',#606,.T.);
#422=FACE_OUTER_BOUND('',#608,.T.);
#423=FACE_OUTER_BOUND('',#609,.T.);
#424=FACE_OUTER_BOUND('',#610,.T.);
#425=FACE_OUTER_BOUND('',#612,.T.);
#426=FACE_OUTER_BOUND('',#613,.T.);
#427=FACE_OUTER_BOUND('',#614,.T.);
#428=FACE_OUTER_BOUND('',#615,.T.);
#429=FACE_OUTER_BOUND('',#616,.T.);
#430=FACE_OUTER_BOUND('',#617,.T.);
#431=FACE_OUTER_BOUND('',#618,.T.);
#432=FACE_OUTER_BOUND('',#619,.T.);
#433=FACE_OUTER_BOUND('',#620,.T.);
#434=FACE_OUTER_BOUND('',#621,.T.);
#435=FACE_OUTER_BOUND('',#622,.T.);
#436=FACE_OUTER_BOUND('',#623,.T.);
#437=FACE_OUTER_BOUND('',#624,.T.);
#438=FACE_OUTER_BOUND('',#625,.T.);
#439=FACE_OUTER_BOUND('',#626,.T.);
#440=FACE_OUTER_BOUND('',#627,.T.);
#441=FACE_OUTER_BOUND('',#628,.T.);
#442=FACE_OUTER_BOUND('',#629,.T.);
#443=FACE_OUTER_BOUND('',#631,.T.);
#444=FACE_OUTER_BOUND('',#632,.T.);
#445=FACE_OUTER_BOUND('',#633,.T.);
#446=FACE_OUTER_BOUND('',#635,.T.);
#447=FACE_OUTER_BOUND('',#636,.T.);
#448=FACE_OUTER_BOUND('',#637,.T.);
#449=FACE_OUTER_BOUND('',#638,.T.);
#450=FACE_OUTER_BOUND('',#640,.T.);
#451=FACE_OUTER_BOUND('',#642,.T.);
#452=FACE_OUTER_BOUND('',#643,.T.);
#453=FACE_OUTER_BOUND('',#644,.T.);
#454=FACE_OUTER_BOUND('',#645,.T.);
#455=FACE_OUTER_BOUND('',#646,.T.);
#456=FACE_OUTER_BOUND('',#647,.T.);
#457=FACE_OUTER_BOUND('',#648,.T.);
#458=FACE_OUTER_BOUND('',#649,.T.);
#459=FACE_OUTER_BOUND('',#651,.T.);
#460=FACE_OUTER_BOUND('',#652,.T.);
#461=FACE_OUTER_BOUND('',#653,.T.);
#462=FACE_OUTER_BOUND('',#654,.T.);
#463=FACE_OUTER_BOUND('',#655,.T.);
#464=FACE_OUTER_BOUND('',#656,.T.);
#465=FACE_OUTER_BOUND('',#657,.T.);
#466=FACE_OUTER_BOUND('',#658,.T.);
#467=FACE_OUTER_BOUND('',#659,.T.);
#468=FACE_OUTER_BOUND('',#661,.T.);
#469=FACE_OUTER_BOUND('',#663,.T.);
#470=FACE_OUTER_BOUND('',#664,.T.);
#471=FACE_OUTER_BOUND('',#665,.T.);
#472=FACE_OUTER_BOUND('',#666,.T.);
#473=FACE_OUTER_BOUND('',#667,.T.);
#474=FACE_OUTER_BOUND('',#668,.T.);
#475=FACE_OUTER_BOUND('',#669,.T.);
#476=FACE_OUTER_BOUND('',#670,.T.);
#477=FACE_OUTER_BOUND('',#671,.T.);
#478=FACE_OUTER_BOUND('',#672,.T.);
#479=FACE_OUTER_BOUND('',#673,.T.);
#480=FACE_OUTER_BOUND('',#675,.T.);
#481=FACE_OUTER_BOUND('',#677,.T.);
#482=FACE_OUTER_BOUND('',#678,.T.);
#483=FACE_OUTER_BOUND('',#679,.T.);
#484=FACE_OUTER_BOUND('',#680,.T.);
#485=FACE_OUTER_BOUND('',#681,.T.);
#486=FACE_OUTER_BOUND('',#682,.T.);
#487=FACE_OUTER_BOUND('',#683,.T.);
#488=FACE_OUTER_BOUND('',#684,.T.);
#489=FACE_OUTER_BOUND('',#685,.T.);
#490=FACE_OUTER_BOUND('',#686,.T.);
#491=FACE_OUTER_BOUND('',#687,.T.);
#492=FACE_OUTER_BOUND('',#688,.T.);
#493=FACE_OUTER_BOUND('',#689,.T.);
#494=FACE_OUTER_BOUND('',#690,.T.);
#495=FACE_OUTER_BOUND('',#691,.T.);
#496=FACE_OUTER_BOUND('',#692,.T.);
#497=FACE_OUTER_BOUND('',#693,.T.);
#498=FACE_OUTER_BOUND('',#694,.T.);
#499=FACE_OUTER_BOUND('',#696,.T.);
#500=FACE_OUTER_BOUND('',#697,.T.);
#501=FACE_OUTER_BOUND('',#698,.T.);
#502=FACE_OUTER_BOUND('',#700,.T.);
#503=FACE_OUTER_BOUND('',#701,.T.);
#504=FACE_OUTER_BOUND('',#702,.T.);
#505=FACE_OUTER_BOUND('',#703,.T.);
#506=FACE_OUTER_BOUND('',#704,.T.);
#507=FACE_OUTER_BOUND('',#705,.T.);
#508=FACE_OUTER_BOUND('',#706,.T.);
#509=FACE_OUTER_BOUND('',#707,.T.);
#510=FACE_OUTER_BOUND('',#708,.T.);
#511=EDGE_LOOP('',(#2152,#2153,#2154,#2155));
#512=EDGE_LOOP('',(#2156,#2157,#2158,#2159));
#513=EDGE_LOOP('',(#2160,#2161,#2162,#2163));
#514=EDGE_LOOP('',(#2164,#2165,#2166,#2167));
#515=EDGE_LOOP('',(#2168,#2169,#2170,#2171));
#516=EDGE_LOOP('',(#2172,#2173,#2174,#2175));
#517=EDGE_LOOP('',(#2176,#2177,#2178,#2179));
#518=EDGE_LOOP('',(#2180,#2181,#2182,#2183));
#519=EDGE_LOOP('',(#2184));
#520=EDGE_LOOP('',(#2185));
#521=EDGE_LOOP('',(#2186));
#522=EDGE_LOOP('',(#2187,#2188,#2189,#2190));
#523=EDGE_LOOP('',(#2191));
#524=EDGE_LOOP('',(#2192));
#525=EDGE_LOOP('',(#2193));
#526=EDGE_LOOP('',(#2194,#2195,#2196));
#527=EDGE_LOOP('',(#2197,#2198,#2199,#2200));
#528=EDGE_LOOP('',(#2201,#2202,#2203,#2204,#2205,#2206,#2207,#2208,#2209,
#2210,#2211,#2212,#2213,#2214));
#529=EDGE_LOOP('',(#2215,#2216,#2217));
#530=EDGE_LOOP('',(#2218,#2219,#2220,#2221));
#531=EDGE_LOOP('',(#2222,#2223,#2224,#2225));
#532=EDGE_LOOP('',(#2226,#2227,#2228,#2229,#2230,#2231));
#533=EDGE_LOOP('',(#2232,#2233,#2234,#2235,#2236));
#534=EDGE_LOOP('',(#2237,#2238,#2239,#2240,#2241,#2242));
#535=EDGE_LOOP('',(#2243,#2244,#2245,#2246,#2247,#2248,#2249,#2250,#2251,
#2252,#2253,#2254));
#536=EDGE_LOOP('',(#2255,#2256,#2257,#2258,#2259,#2260,#2261,#2262,#2263,
#2264,#2265,#2266,#2267,#2268,#2269,#2270,#2271,#2272,#2273,#2274,#2275,
#2276,#2277,#2278,#2279,#2280,#2281));
#537=EDGE_LOOP('',(#2282,#2283,#2284,#2285));
#538=EDGE_LOOP('',(#2286,#2287,#2288,#2289));
#539=EDGE_LOOP('',(#2290,#2291,#2292,#2293));
#540=EDGE_LOOP('',(#2294,#2295,#2296,#2297,#2298,#2299));
#541=EDGE_LOOP('',(#2300,#2301,#2302,#2303));
#542=EDGE_LOOP('',(#2304,#2305,#2306,#2307));
#543=EDGE_LOOP('',(#2308,#2309,#2310,#2311));
#544=EDGE_LOOP('',(#2312,#2313,#2314,#2315));
#545=EDGE_LOOP('',(#2316,#2317,#2318,#2319));
#546=EDGE_LOOP('',(#2320,#2321,#2322,#2323));
#547=EDGE_LOOP('',(#2324,#2325,#2326,#2327));
#548=EDGE_LOOP('',(#2328,#2329,#2330,#2331,#2332,#2333));
#549=EDGE_LOOP('',(#2334,#2335,#2336,#2337,#2338));
#550=EDGE_LOOP('',(#2339,#2340,#2341,#2342));
#551=EDGE_LOOP('',(#2343,#2344,#2345,#2346));
#552=EDGE_LOOP('',(#2347,#2348,#2349,#2350));
#553=EDGE_LOOP('',(#2351,#2352,#2353,#2354));
#554=EDGE_LOOP('',(#2355,#2356,#2357,#2358));
#555=EDGE_LOOP('',(#2359,#2360,#2361,#2362));
#556=EDGE_LOOP('',(#2363,#2364,#2365,#2366));
#557=EDGE_LOOP('',(#2367,#2368,#2369,#2370));
#558=EDGE_LOOP('',(#2371,#2372,#2373,#2374));
#559=EDGE_LOOP('',(#2375,#2376,#2377,#2378));
#560=EDGE_LOOP('',(#2379,#2380,#2381,#2382));
#561=EDGE_LOOP('',(#2383,#2384,#2385,#2386));
#562=EDGE_LOOP('',(#2387,#2388,#2389,#2390));
#563=EDGE_LOOP('',(#2391,#2392,#2393,#2394));
#564=EDGE_LOOP('',(#2395,#2396,#2397,#2398));
#565=EDGE_LOOP('',(#2399,#2400,#2401,#2402));
#566=EDGE_LOOP('',(#2403,#2404,#2405,#2406));
#567=EDGE_LOOP('',(#2407,#2408,#2409,#2410));
#568=EDGE_LOOP('',(#2411,#2412,#2413,#2414));
#569=EDGE_LOOP('',(#2415,#2416,#2417,#2418,#2419,#2420,#2421,#2422));
#570=EDGE_LOOP('',(#2423,#2424,#2425,#2426));
#571=EDGE_LOOP('',(#2427,#2428,#2429,#2430));
#572=EDGE_LOOP('',(#2431,#2432,#2433,#2434));
#573=EDGE_LOOP('',(#2435,#2436,#2437,#2438));
#574=EDGE_LOOP('',(#2439,#2440,#2441,#2442));
#575=EDGE_LOOP('',(#2443,#2444,#2445,#2446));
#576=EDGE_LOOP('',(#2447,#2448,#2449,#2450));
#577=EDGE_LOOP('',(#2451,#2452,#2453,#2454));
#578=EDGE_LOOP('',(#2455,#2456,#2457,#2458,#2459,#2460,#2461,#2462,#2463,
#2464,#2465,#2466,#2467,#2468,#2469,#2470,#2471,#2472,#2473,#2474,#2475,
#2476,#2477,#2478,#2479,#2480,#2481,#2482,#2483,#2484,#2485,#2486,#2487,
#2488,#2489,#2490,#2491,#2492,#2493,#2494,#2495,#2496,#2497,#2498));
#579=EDGE_LOOP('',(#2499));
#580=EDGE_LOOP('',(#2500,#2501,#2502,#2503,#2504,#2505,#2506,#2507,#2508,
#2509,#2510,#2511));
#581=EDGE_LOOP('',(#2512,#2513,#2514,#2515,#2516,#2517));
#582=EDGE_LOOP('',(#2518,#2519,#2520,#2521));
#583=EDGE_LOOP('',(#2522,#2523,#2524,#2525));
#584=EDGE_LOOP('',(#2526,#2527,#2528,#2529,#2530,#2531));
#585=EDGE_LOOP('',(#2532,#2533,#2534,#2535,#2536,#2537,#2538,#2539,#2540,
#2541,#2542,#2543));
#586=EDGE_LOOP('',(#2544));
#587=EDGE_LOOP('',(#2545,#2546,#2547,#2548,#2549,#2550,#2551,#2552,#2553,
#2554));
#588=EDGE_LOOP('',(#2555));
#589=EDGE_LOOP('',(#2556,#2557,#2558));
#590=EDGE_LOOP('',(#2559,#2560,#2561,#2562));
#591=EDGE_LOOP('',(#2563,#2564,#2565,#2566));
#592=EDGE_LOOP('',(#2567,#2568,#2569,#2570));
#593=EDGE_LOOP('',(#2571,#2572,#2573,#2574));
#594=EDGE_LOOP('',(#2575,#2576,#2577));
#595=EDGE_LOOP('',(#2578,#2579,#2580,#2581,#2582,#2583,#2584,#2585,#2586,
#2587,#2588,#2589));
#596=EDGE_LOOP('',(#2590));
#597=EDGE_LOOP('',(#2591,#2592,#2593,#2594));
#598=EDGE_LOOP('',(#2595,#2596,#2597));
#599=EDGE_LOOP('',(#2598,#2599,#2600,#2601,#2602,#2603,#2604,#2605));
#600=EDGE_LOOP('',(#2606,#2607,#2608,#2609,#2610,#2611,#2612,#2613,#2614,
#2615));
#601=EDGE_LOOP('',(#2616));
#602=EDGE_LOOP('',(#2617,#2618,#2619,#2620));
#603=EDGE_LOOP('',(#2621,#2622,#2623,#2624));
#604=EDGE_LOOP('',(#2625,#2626,#2627,#2628,#2629,#2630,#2631));
#605=EDGE_LOOP('',(#2632));
#606=EDGE_LOOP('',(#2633));
#607=EDGE_LOOP('',(#2634,#2635,#2636,#2637,#2638,#2639));
#608=EDGE_LOOP('',(#2640,#2641,#2642,#2643));
#609=EDGE_LOOP('',(#2644,#2645,#2646,#2647));
#610=EDGE_LOOP('',(#2648));
#611=EDGE_LOOP('',(#2649));
#612=EDGE_LOOP('',(#2650,#2651,#2652,#2653));
#613=EDGE_LOOP('',(#2654,#2655,#2656,#2657));
#614=EDGE_LOOP('',(#2658,#2659,#2660,#2661));
#615=EDGE_LOOP('',(#2662,#2663,#2664,#2665));
#616=EDGE_LOOP('',(#2666,#2667,#2668,#2669));
#617=EDGE_LOOP('',(#2670,#2671,#2672,#2673));
#618=EDGE_LOOP('',(#2674,#2675,#2676,#2677));
#619=EDGE_LOOP('',(#2678,#2679,#2680,#2681));
#620=EDGE_LOOP('',(#2682,#2683,#2684,#2685,#2686,#2687));
#621=EDGE_LOOP('',(#2688,#2689,#2690,#2691));
#622=EDGE_LOOP('',(#2692));
#623=EDGE_LOOP('',(#2693,#2694,#2695,#2696));
#624=EDGE_LOOP('',(#2697,#2698,#2699,#2700));
#625=EDGE_LOOP('',(#2701,#2702,#2703,#2704));
#626=EDGE_LOOP('',(#2705,#2706,#2707,#2708));
#627=EDGE_LOOP('',(#2709,#2710,#2711,#2712));
#628=EDGE_LOOP('',(#2713,#2714,#2715,#2716));
#629=EDGE_LOOP('',(#2717));
#630=EDGE_LOOP('',(#2718,#2719,#2720,#2721));
#631=EDGE_LOOP('',(#2722,#2723));
#632=EDGE_LOOP('',(#2724,#2725));
#633=EDGE_LOOP('',(#2726,#2727,#2728));
#634=EDGE_LOOP('',(#2729,#2730));
#635=EDGE_LOOP('',(#2731));
#636=EDGE_LOOP('',(#2732,#2733,#2734,#2735));
#637=EDGE_LOOP('',(#2736,#2737,#2738,#2739));
#638=EDGE_LOOP('',(#2740));
#639=EDGE_LOOP('',(#2741));
#640=EDGE_LOOP('',(#2742,#2743,#2744,#2745,#2746,#2747));
#641=EDGE_LOOP('',(#2748));
#642=EDGE_LOOP('',(#2749,#2750,#2751,#2752));
#643=EDGE_LOOP('',(#2753,#2754,#2755,#2756));
#644=EDGE_LOOP('',(#2757,#2758,#2759,#2760));
#645=EDGE_LOOP('',(#2761,#2762,#2763,#2764));
#646=EDGE_LOOP('',(#2765,#2766,#2767,#2768));
#647=EDGE_LOOP('',(#2769,#2770,#2771,#2772));
#648=EDGE_LOOP('',(#2773,#2774,#2775,#2776));
#649=EDGE_LOOP('',(#2777,#2778,#2779,#2780,#2781,#2782));
#650=EDGE_LOOP('',(#2783));
#651=EDGE_LOOP('',(#2784,#2785,#2786,#2787));
#652=EDGE_LOOP('',(#2788,#2789,#2790,#2791));
#653=EDGE_LOOP('',(#2792));
#654=EDGE_LOOP('',(#2793,#2794,#2795));
#655=EDGE_LOOP('',(#2796,#2797,#2798,#2799));
#656=EDGE_LOOP('',(#2800));
#657=EDGE_LOOP('',(#2801));
#658=EDGE_LOOP('',(#2802,#2803,#2804,#2805));
#659=EDGE_LOOP('',(#2806));
#660=EDGE_LOOP('',(#2807));
#661=EDGE_LOOP('',(#2808));
#662=EDGE_LOOP('',(#2809));
#663=EDGE_LOOP('',(#2810,#2811,#2812,#2813));
#664=EDGE_LOOP('',(#2814,#2815,#2816,#2817,#2818,#2819,#2820,#2821,#2822));
#665=EDGE_LOOP('',(#2823,#2824,#2825,#2826,#2827,#2828,#2829,#2830,#2831));
#666=EDGE_LOOP('',(#2832,#2833,#2834,#2835));
#667=EDGE_LOOP('',(#2836,#2837,#2838,#2839));
#668=EDGE_LOOP('',(#2840,#2841,#2842,#2843));
#669=EDGE_LOOP('',(#2844,#2845,#2846,#2847));
#670=EDGE_LOOP('',(#2848,#2849,#2850,#2851));
#671=EDGE_LOOP('',(#2852,#2853,#2854,#2855));
#672=EDGE_LOOP('',(#2856,#2857,#2858,#2859));
#673=EDGE_LOOP('',(#2860));
#674=EDGE_LOOP('',(#2861));
#675=EDGE_LOOP('',(#2862));
#676=EDGE_LOOP('',(#2863));
#677=EDGE_LOOP('',(#2864,#2865,#2866,#2867));
#678=EDGE_LOOP('',(#2868,#2869,#2870,#2871));
#679=EDGE_LOOP('',(#2872,#2873,#2874,#2875));
#680=EDGE_LOOP('',(#2876,#2877,#2878,#2879));
#681=EDGE_LOOP('',(#2880,#2881,#2882,#2883));
#682=EDGE_LOOP('',(#2884,#2885,#2886,#2887));
#683=EDGE_LOOP('',(#2888,#2889,#2890,#2891,#2892,#2893));
#684=EDGE_LOOP('',(#2894,#2895,#2896,#2897,#2898,#2899));
#685=EDGE_LOOP('',(#2900,#2901,#2902,#2903,#2904,#2905));
#686=EDGE_LOOP('',(#2906,#2907,#2908,#2909,#2910,#2911,#2912,#2913));
#687=EDGE_LOOP('',(#2914,#2915,#2916,#2917));
#688=EDGE_LOOP('',(#2918,#2919,#2920,#2921));
#689=EDGE_LOOP('',(#2922,#2923,#2924,#2925,#2926,#2927));
#690=EDGE_LOOP('',(#2928,#2929,#2930,#2931));
#691=EDGE_LOOP('',(#2932,#2933,#2934,#2935,#2936,#2937));
#692=EDGE_LOOP('',(#2938,#2939,#2940,#2941,#2942,#2943,#2944,#2945,#2946,
#2947));
#693=EDGE_LOOP('',(#2948));
#694=EDGE_LOOP('',(#2949));
#695=EDGE_LOOP('',(#2950,#2951,#2952,#2953,#2954,#2955));
#696=EDGE_LOOP('',(#2956,#2957,#2958,#2959));
#697=EDGE_LOOP('',(#2960,#2961,#2962,#2963));
#698=EDGE_LOOP('',(#2964));
#699=EDGE_LOOP('',(#2965));
#700=EDGE_LOOP('',(#2966,#2967,#2968,#2969));
#701=EDGE_LOOP('',(#2970,#2971,#2972,#2973));
#702=EDGE_LOOP('',(#2974,#2975,#2976,#2977));
#703=EDGE_LOOP('',(#2978,#2979,#2980,#2981));
#704=EDGE_LOOP('',(#2982,#2983,#2984,#2985));
#705=EDGE_LOOP('',(#2986,#2987,#2988,#2989));
#706=EDGE_LOOP('',(#2990,#2991,#2992,#2993));
#707=EDGE_LOOP('',(#2994,#2995,#2996,#2997));
#708=EDGE_LOOP('',(#2998,#2999,#3000,#3001,#3002,#3003));
#709=LINE('',#4537,#1040);
#710=LINE('',#4543,#1041);
#711=LINE('',#4549,#1042);
#712=LINE('',#4554,#1043);
#713=LINE('',#4556,#1044);
#714=LINE('',#4558,#1045);
#715=LINE('',#4559,#1046);
#716=LINE('',#4562,#1047);
#717=LINE('',#4564,#1048);
#718=LINE('',#4565,#1049);
#719=LINE('',#4568,#1050);
#720=LINE('',#4570,#1051);
#721=LINE('',#4571,#1052);
#722=LINE('',#4573,#1053);
#723=LINE('',#4574,#1054);
#724=LINE('',#4581,#1055);
#725=LINE('',#4584,#1056);
#726=LINE('',#4588,#1057);
#727=LINE('',#4592,#1058);
#728=LINE('',#4593,#1059);
#729=LINE('',#4601,#1060);
#730=LINE('',#4605,#1061);
#731=LINE('',#4615,#1062);
#732=LINE('',#4618,#1063);
#733=LINE('',#4624,#1064);
#734=LINE('',#4625,#1065);
#735=LINE('',#4628,#1066);
#736=LINE('',#4630,#1067);
#737=LINE('',#4631,#1068);
#738=LINE('',#4634,#1069);
#739=LINE('',#4636,#1070);
#740=LINE('',#4637,#1071);
#741=LINE('',#4640,#1072);
#742=LINE('',#4642,#1073);
#743=LINE('',#4643,#1074);
#744=LINE('',#4646,#1075);
#745=LINE('',#4648,#1076);
#746=LINE('',#4650,#1077);
#747=LINE('',#4651,#1078);
#748=LINE('',#4654,#1079);
#749=LINE('',#4656,#1080);
#750=LINE('',#4657,#1081);
#751=LINE('',#4660,#1082);
#752=LINE('',#4662,#1083);
#753=LINE('',#4664,#1084);
#754=LINE('',#4666,#1085);
#755=LINE('',#4668,#1086);
#756=LINE('',#4670,#1087);
#757=LINE('',#4672,#1088);
#758=LINE('',#4673,#1089);
#759=LINE('',#4676,#1090);
#760=LINE('',#4678,#1091);
#761=LINE('',#4680,#1092);
#762=LINE('',#4682,#1093);
#763=LINE('',#4684,#1094);
#764=LINE('',#4686,#1095);
#765=LINE('',#4688,#1096);
#766=LINE('',#4690,#1097);
#767=LINE('',#4692,#1098);
#768=LINE('',#4694,#1099);
#769=LINE('',#4696,#1100);
#770=LINE('',#4698,#1101);
#771=LINE('',#4700,#1102);
#772=LINE('',#4702,#1103);
#773=LINE('',#4704,#1104);
#774=LINE('',#4706,#1105);
#775=LINE('',#4708,#1106);
#776=LINE('',#4710,#1107);
#777=LINE('',#4712,#1108);
#778=LINE('',#4714,#1109);
#779=LINE('',#4716,#1110);
#780=LINE('',#4717,#1111);
#781=LINE('',#4724,#1112);
#782=LINE('',#4726,#1113);
#783=LINE('',#4728,#1114);
#784=LINE('',#4729,#1115);
#785=LINE('',#4732,#1116);
#786=LINE('',#4734,#1117);
#787=LINE('',#4735,#1118);
#788=LINE('',#4738,#1119);
#789=LINE('',#4740,#1120);
#790=LINE('',#4741,#1121);
#791=LINE('',#4743,#1122);
#792=LINE('',#4744,#1123);
#793=LINE('',#4747,#1124);
#794=LINE('',#4748,#1125);
#795=LINE('',#4751,#1126);
#796=LINE('',#4752,#1127);
#797=LINE('',#4755,#1128);
#798=LINE('',#4756,#1129);
#799=LINE('',#4759,#1130);
#800=LINE('',#4761,#1131);
#801=LINE('',#4762,#1132);
#802=LINE('',#4765,#1133);
#803=LINE('',#4766,#1134);
#804=LINE('',#4769,#1135);
#805=LINE('',#4770,#1136);
#806=LINE('',#4773,#1137);
#807=LINE('',#4774,#1138);
#808=LINE('',#4777,#1139);
#809=LINE('',#4778,#1140);
#810=LINE('',#4781,#1141);
#811=LINE('',#4783,#1142);
#812=LINE('',#4784,#1143);
#813=LINE('',#4787,#1144);
#814=LINE('',#4789,#1145);
#815=LINE('',#4790,#1146);
#816=LINE('',#4793,#1147);
#817=LINE('',#4795,#1148);
#818=LINE('',#4796,#1149);
#819=LINE('',#4799,#1150);
#820=LINE('',#4801,#1151);
#821=LINE('',#4802,#1152);
#822=LINE('',#4805,#1153);
#823=LINE('',#4807,#1154);
#824=LINE('',#4808,#1155);
#825=LINE('',#4811,#1156);
#826=LINE('',#4812,#1157);
#827=LINE('',#4815,#1158);
#828=LINE('',#4816,#1159);
#829=LINE('',#4819,#1160);
#830=LINE('',#4820,#1161);
#831=LINE('',#4823,#1162);
#832=LINE('',#4824,#1163);
#833=LINE('',#4827,#1164);
#834=LINE('',#4828,#1165);
#835=LINE('',#4831,#1166);
#836=LINE('',#4832,#1167);
#837=LINE('',#4835,#1168);
#838=LINE('',#4836,#1169);
#839=LINE('',#4839,#1170);
#840=LINE('',#4840,#1171);
#841=LINE('',#4843,#1172);
#842=LINE('',#4845,#1173);
#843=LINE('',#4846,#1174);
#844=LINE('',#4849,#1175);
#845=LINE('',#4850,#1176);
#846=LINE('',#4852,#1177);
#847=LINE('',#4855,#1178);
#848=LINE('',#4856,#1179);
#849=LINE('',#4859,#1180);
#850=LINE('',#4860,#1181);
#851=LINE('',#4863,#1182);
#852=LINE('',#4864,#1183);
#853=LINE('',#4867,#1184);
#854=LINE('',#4868,#1185);
#855=LINE('',#4871,#1186);
#856=LINE('',#4875,#1187);
#857=LINE('',#4876,#1188);
#858=LINE('',#4879,#1189);
#859=LINE('',#4881,#1190);
#860=LINE('',#4882,#1191);
#861=LINE('',#4884,#1192);
#862=LINE('',#4885,#1193);
#863=LINE('',#4888,#1194);
#864=LINE('',#4889,#1195);
#865=LINE('',#4891,#1196);
#866=LINE('',#4894,#1197);
#867=LINE('',#4895,#1198);
#868=LINE('',#4897,#1199);
#869=LINE('',#4899,#1200);
#870=LINE('',#4906,#1201);
#871=LINE('',#4910,#1202);
#872=LINE('',#4912,#1203);
#873=LINE('',#4915,#1204);
#874=LINE('',#4918,#1205);
#875=LINE('',#4920,#1206);
#876=LINE('',#4924,#1207);
#877=LINE('',#4927,#1208);
#878=LINE('',#4930,#1209);
#879=LINE('',#4931,#1210);
#880=LINE('',#4933,#1211);
#881=LINE('',#4934,#1212);
#882=LINE('',#4937,#1213);
#883=LINE('',#4939,#1214);
#884=LINE('',#4941,#1215);
#885=LINE('',#4943,#1216);
#886=LINE('',#4945,#1217);
#887=LINE('',#4947,#1218);
#888=LINE('',#4949,#1219);
#889=LINE('',#4951,#1220);
#890=LINE('',#4952,#1221);
#891=LINE('',#4957,#1222);
#892=LINE('',#4959,#1223);
#893=LINE('',#4961,#1224);
#894=LINE('',#4963,#1225);
#895=LINE('',#4965,#1226);
#896=LINE('',#4967,#1227);
#897=LINE('',#4968,#1228);
#898=LINE('',#4973,#1229);
#899=LINE('',#4977,#1230);
#900=LINE('',#4981,#1231);
#901=LINE('',#4986,#1232);
#902=LINE('',#4989,#1233);
#903=LINE('',#4991,#1234);
#904=LINE('',#4992,#1235);
#905=LINE('',#4994,#1236);
#906=LINE('',#4997,#1237);
#907=LINE('',#4999,#1238);
#908=LINE('',#5001,#1239);
#909=LINE('',#5003,#1240);
#910=LINE('',#5004,#1241);
#911=LINE('',#5006,#1242);
#912=LINE('',#5007,#1243);
#913=LINE('',#5011,#1244);
#914=LINE('',#5012,#1245);
#915=LINE('',#5013,#1246);
#916=LINE('',#5016,#1247);
#917=LINE('',#5017,#1248);
#918=LINE('',#5019,#1249);
#919=LINE('',#5021,#1250);
#920=LINE('',#5032,#1251);
#921=LINE('',#5034,#1252);
#922=LINE('',#5036,#1253);
#923=LINE('',#5038,#1254);
#924=LINE('',#5040,#1255);
#925=LINE('',#5041,#1256);
#926=LINE('',#5045,#1257);
#927=LINE('',#5049,#1258);
#928=LINE('',#5056,#1259);
#929=LINE('',#5058,#1260);
#930=LINE('',#5062,#1261);
#931=LINE('',#5063,#1262);
#932=LINE('',#5064,#1263);
#933=LINE('',#5067,#1264);
#934=LINE('',#5068,#1265);
#935=LINE('',#5071,#1266);
#936=LINE('',#5072,#1267);
#937=LINE('',#5075,#1268);
#938=LINE('',#5076,#1269);
#939=LINE('',#5079,#1270);
#940=LINE('',#5080,#1271);
#941=LINE('',#5082,#1272);
#942=LINE('',#5090,#1273);
#943=LINE('',#5096,#1274);
#944=LINE('',#5100,#1275);
#945=LINE('',#5102,#1276);
#946=LINE('',#5104,#1277);
#947=LINE('',#5105,#1278);
#948=LINE('',#5110,#1279);
#949=LINE('',#5115,#1280);
#950=LINE('',#5119,#1281);
#951=LINE('',#5121,#1282);
#952=LINE('',#5128,#1283);
#953=LINE('',#5142,#1284);
#954=LINE('',#5146,#1285);
#955=LINE('',#5152,#1286);
#956=LINE('',#5154,#1287);
#957=LINE('',#5156,#1288);
#958=LINE('',#5158,#1289);
#959=LINE('',#5160,#1290);
#960=LINE('',#5161,#1291);
#961=LINE('',#5167,#1292);
#962=LINE('',#5168,#1293);
#963=LINE('',#5169,#1294);
#964=LINE('',#5172,#1295);
#965=LINE('',#5173,#1296);
#966=LINE('',#5176,#1297);
#967=LINE('',#5177,#1298);
#968=LINE('',#5180,#1299);
#969=LINE('',#5181,#1300);
#970=LINE('',#5184,#1301);
#971=LINE('',#5185,#1302);
#972=LINE('',#5187,#1303);
#973=LINE('',#5192,#1304);
#974=LINE('',#5198,#1305);
#975=LINE('',#5202,#1306);
#976=LINE('',#5211,#1307);
#977=LINE('',#5223,#1308);
#978=LINE('',#5233,#1309);
#979=LINE('',#5246,#1310);
#980=LINE('',#5267,#1311);
#981=LINE('',#5292,#1312);
#982=LINE('',#5293,#1313);
#983=LINE('',#5295,#1314);
#984=LINE('',#5297,#1315);
#985=LINE('',#5301,#1316);
#986=LINE('',#5303,#1317);
#987=LINE('',#5305,#1318);
#988=LINE('',#5317,#1319);
#989=LINE('',#5322,#1320);
#990=LINE('',#5330,#1321);
#991=LINE('',#5332,#1322);
#992=LINE('',#5333,#1323);
#993=LINE('',#5336,#1324);
#994=LINE('',#5338,#1325);
#995=LINE('',#5339,#1326);
#996=LINE('',#5342,#1327);
#997=LINE('',#5344,#1328);
#998=LINE('',#5345,#1329);
#999=LINE('',#5348,#1330);
#1000=LINE('',#5350,#1331);
#1001=LINE('',#5351,#1332);
#1002=LINE('',#5354,#1333);
#1003=LINE('',#5356,#1334);
#1004=LINE('',#5362,#1335);
#1005=LINE('',#5363,#1336);
#1006=LINE('',#5367,#1337);
#1007=LINE('',#5369,#1338);
#1008=LINE('',#5371,#1339);
#1009=LINE('',#5373,#1340);
#1010=LINE('',#5376,#1341);
#1011=LINE('',#5382,#1342);
#1012=LINE('',#5384,#1343);
#1013=LINE('',#5387,#1344);
#1014=LINE('',#5388,#1345);
#1015=LINE('',#5391,#1346);
#1016=LINE('',#5392,#1347);
#1017=LINE('',#5394,#1348);
#1018=LINE('',#5405,#1349);
#1019=LINE('',#5407,#1350);
#1020=LINE('',#5409,#1351);
#1021=LINE('',#5411,#1352);
#1022=LINE('',#5413,#1353);
#1023=LINE('',#5414,#1354);
#1024=LINE('',#5418,#1355);
#1025=LINE('',#5422,#1356);
#1026=LINE('',#5429,#1357);
#1027=LINE('',#5431,#1358);
#1028=LINE('',#5435,#1359);
#1029=LINE('',#5436,#1360);
#1030=LINE('',#5437,#1361);
#1031=LINE('',#5440,#1362);
#1032=LINE('',#5441,#1363);
#1033=LINE('',#5444,#1364);
#1034=LINE('',#5445,#1365);
#1035=LINE('',#5448,#1366);
#1036=LINE('',#5449,#1367);
#1037=LINE('',#5452,#1368);
#1038=LINE('',#5453,#1369);
#1039=LINE('',#5455,#1370);
#1040=VECTOR('',#3626,0.275);
#1041=VECTOR('',#3633,0.275);
#1042=VECTOR('',#3640,0.34);
#1043=VECTOR('',#3645,1.);
#1044=VECTOR('',#3646,1.);
#1045=VECTOR('',#3647,1.);
#1046=VECTOR('',#3648,1.);
#1047=VECTOR('',#3651,1.);
#1048=VECTOR('',#3652,1.);
#1049=VECTOR('',#3653,1.);
#1050=VECTOR('',#3656,1.);
#1051=VECTOR('',#3657,1.);
#1052=VECTOR('',#3658,1.);
#1053=VECTOR('',#3661,1.);
#1054=VECTOR('',#3662,1.);
#1055=VECTOR('',#3671,1.);
#1056=VECTOR('',#3674,1.);
#1057=VECTOR('',#3677,1.);
#1058=VECTOR('',#3680,1.);
#1059=VECTOR('',#3681,1.);
#1060=VECTOR('',#3688,1.);
#1061=VECTOR('',#3691,1.);
#1062=VECTOR('',#3694,1.);
#1063=VECTOR('',#3697,1.);
#1064=VECTOR('',#3704,1.);
#1065=VECTOR('',#3705,1.);
#1066=VECTOR('',#3708,1.);
#1067=VECTOR('',#3709,1.);
#1068=VECTOR('',#3710,1.);
#1069=VECTOR('',#3713,1.);
#1070=VECTOR('',#3714,1.);
#1071=VECTOR('',#3715,1.);
#1072=VECTOR('',#3718,1.);
#1073=VECTOR('',#3719,1.);
#1074=VECTOR('',#3720,1.);
#1075=VECTOR('',#3723,1.);
#1076=VECTOR('',#3724,1.);
#1077=VECTOR('',#3725,1.);
#1078=VECTOR('',#3726,1.);
#1079=VECTOR('',#3729,1.);
#1080=VECTOR('',#3730,1.);
#1081=VECTOR('',#3731,1.);
#1082=VECTOR('',#3734,1.);
#1083=VECTOR('',#3735,1.);
#1084=VECTOR('',#3736,1.);
#1085=VECTOR('',#3737,1.);
#1086=VECTOR('',#3738,1.);
#1087=VECTOR('',#3739,1.);
#1088=VECTOR('',#3740,1.);
#1089=VECTOR('',#3741,1.);
#1090=VECTOR('',#3744,1.);
#1091=VECTOR('',#3745,1.);
#1092=VECTOR('',#3746,1.);
#1093=VECTOR('',#3747,1.);
#1094=VECTOR('',#3748,1.);
#1095=VECTOR('',#3749,1.);
#1096=VECTOR('',#3750,1.);
#1097=VECTOR('',#3751,1.);
#1098=VECTOR('',#3752,1.);
#1099=VECTOR('',#3753,1.);
#1100=VECTOR('',#3754,1.);
#1101=VECTOR('',#3755,1.);
#1102=VECTOR('',#3756,1.);
#1103=VECTOR('',#3757,1.);
#1104=VECTOR('',#3758,1.);
#1105=VECTOR('',#3759,1.);
#1106=VECTOR('',#3760,1.);
#1107=VECTOR('',#3761,1.);
#1108=VECTOR('',#3762,1.);
#1109=VECTOR('',#3763,1.);
#1110=VECTOR('',#3764,1.);
#1111=VECTOR('',#3765,1.);
#1112=VECTOR('',#3772,1.);
#1113=VECTOR('',#3773,1.);
#1114=VECTOR('',#3774,1.);
#1115=VECTOR('',#3775,1.);
#1116=VECTOR('',#3778,1.);
#1117=VECTOR('',#3779,1.);
#1118=VECTOR('',#3780,1.);
#1119=VECTOR('',#3783,1.);
#1120=VECTOR('',#3784,1.);
#1121=VECTOR('',#3785,1.);
#1122=VECTOR('',#3788,1.);
#1123=VECTOR('',#3789,1.);
#1124=VECTOR('',#3792,1.);
#1125=VECTOR('',#3793,1.);
#1126=VECTOR('',#3796,1.);
#1127=VECTOR('',#3797,1.);
#1128=VECTOR('',#3800,1.);
#1129=VECTOR('',#3801,1.);
#1130=VECTOR('',#3804,1.);
#1131=VECTOR('',#3805,1.);
#1132=VECTOR('',#3806,1.);
#1133=VECTOR('',#3809,1.);
#1134=VECTOR('',#3810,1.);
#1135=VECTOR('',#3813,1.);
#1136=VECTOR('',#3814,1.);
#1137=VECTOR('',#3817,1.);
#1138=VECTOR('',#3818,1.);
#1139=VECTOR('',#3821,1.);
#1140=VECTOR('',#3822,1.);
#1141=VECTOR('',#3825,1.);
#1142=VECTOR('',#3826,1.);
#1143=VECTOR('',#3827,1.);
#1144=VECTOR('',#3830,1.);
#1145=VECTOR('',#3831,1.);
#1146=VECTOR('',#3832,1.);
#1147=VECTOR('',#3835,1.);
#1148=VECTOR('',#3836,1.);
#1149=VECTOR('',#3837,1.);
#1150=VECTOR('',#3840,1.);
#1151=VECTOR('',#3841,1.);
#1152=VECTOR('',#3842,1.);
#1153=VECTOR('',#3845,1.);
#1154=VECTOR('',#3846,1.);
#1155=VECTOR('',#3847,1.);
#1156=VECTOR('',#3850,1.);
#1157=VECTOR('',#3851,1.);
#1158=VECTOR('',#3854,1.);
#1159=VECTOR('',#3855,1.);
#1160=VECTOR('',#3858,1.);
#1161=VECTOR('',#3859,1.);
#1162=VECTOR('',#3862,1.);
#1163=VECTOR('',#3863,1.);
#1164=VECTOR('',#3866,1.);
#1165=VECTOR('',#3867,1.);
#1166=VECTOR('',#3870,1.);
#1167=VECTOR('',#3871,1.);
#1168=VECTOR('',#3874,1.);
#1169=VECTOR('',#3875,1.);
#1170=VECTOR('',#3878,1.);
#1171=VECTOR('',#3879,1.);
#1172=VECTOR('',#3882,1.);
#1173=VECTOR('',#3883,1.);
#1174=VECTOR('',#3884,1.);
#1175=VECTOR('',#3887,1.);
#1176=VECTOR('',#3888,1.);
#1177=VECTOR('',#3891,1.);
#1178=VECTOR('',#3894,1.);
#1179=VECTOR('',#3895,1.);
#1180=VECTOR('',#3898,1.);
#1181=VECTOR('',#3899,1.);
#1182=VECTOR('',#3902,1.);
#1183=VECTOR('',#3903,1.);
#1184=VECTOR('',#3906,1.);
#1185=VECTOR('',#3907,1.);
#1186=VECTOR('',#3910,0.21);
#1187=VECTOR('',#3915,1.);
#1188=VECTOR('',#3916,1.);
#1189=VECTOR('',#3919,1.);
#1190=VECTOR('',#3920,1.);
#1191=VECTOR('',#3921,1.);
#1192=VECTOR('',#3924,1.);
#1193=VECTOR('',#3925,1.);
#1194=VECTOR('',#3928,1.);
#1195=VECTOR('',#3929,1.);
#1196=VECTOR('',#3932,1.);
#1197=VECTOR('',#3935,1.);
#1198=VECTOR('',#3936,1.);
#1199=VECTOR('',#3939,1.);
#1200=VECTOR('',#3942,1.);
#1201=VECTOR('',#3951,1.);
#1202=VECTOR('',#3954,1.);
#1203=VECTOR('',#3955,1.);
#1204=VECTOR('',#3958,1.);
#1205=VECTOR('',#3961,1.);
#1206=VECTOR('',#3962,1.);
#1207=VECTOR('',#3967,1.);
#1208=VECTOR('',#3970,1.);
#1209=VECTOR('',#3973,1.);
#1210=VECTOR('',#3974,1.);
#1211=VECTOR('',#3975,1.);
#1212=VECTOR('',#3976,1.);
#1213=VECTOR('',#3979,1.);
#1214=VECTOR('',#3980,1.);
#1215=VECTOR('',#3981,1.);
#1216=VECTOR('',#3982,1.);
#1217=VECTOR('',#3983,1.);
#1218=VECTOR('',#3984,1.);
#1219=VECTOR('',#3985,1.);
#1220=VECTOR('',#3986,1.);
#1221=VECTOR('',#3987,1.);
#1222=VECTOR('',#3992,1.);
#1223=VECTOR('',#3993,1.);
#1224=VECTOR('',#3994,1.);
#1225=VECTOR('',#3995,1.);
#1226=VECTOR('',#3996,1.);
#1227=VECTOR('',#3997,1.);
#1228=VECTOR('',#3998,1.);
#1229=VECTOR('',#4003,1.);
#1230=VECTOR('',#4008,1.);
#1231=VECTOR('',#4013,0.275);
#1232=VECTOR('',#4020,0.275);
#1233=VECTOR('',#4023,1.);
#1234=VECTOR('',#4024,1.);
#1235=VECTOR('',#4025,1.);
#1236=VECTOR('',#4028,1.);
#1237=VECTOR('',#4031,1.);
#1238=VECTOR('',#4032,1.);
#1239=VECTOR('',#4033,1.);
#1240=VECTOR('',#4034,1.);
#1241=VECTOR('',#4035,1.);
#1242=VECTOR('',#4038,1.);
#1243=VECTOR('',#4039,1.);
#1244=VECTOR('',#4044,1.);
#1245=VECTOR('',#4045,1.);
#1246=VECTOR('',#4046,1.);
#1247=VECTOR('',#4049,1.);
#1248=VECTOR('',#4050,1.);
#1249=VECTOR('',#4053,1.);
#1250=VECTOR('',#4056,1.);
#1251=VECTOR('',#4069,1.);
#1252=VECTOR('',#4070,1.);
#1253=VECTOR('',#4071,1.);
#1254=VECTOR('',#4072,1.);
#1255=VECTOR('',#4073,1.);
#1256=VECTOR('',#4074,1.);
#1257=VECTOR('',#4079,0.425);
#1258=VECTOR('',#4084,0.41);
#1259=VECTOR('',#4093,0.26);
#1260=VECTOR('',#4096,0.25);
#1261=VECTOR('',#4099,1.);
#1262=VECTOR('',#4100,1.);
#1263=VECTOR('',#4101,1.);
#1264=VECTOR('',#4104,1.);
#1265=VECTOR('',#4105,1.);
#1266=VECTOR('',#4108,1.);
#1267=VECTOR('',#4109,1.);
#1268=VECTOR('',#4112,1.);
#1269=VECTOR('',#4113,1.);
#1270=VECTOR('',#4116,1.);
#1271=VECTOR('',#4117,1.);
#1272=VECTOR('',#4120,1.);
#1273=VECTOR('',#4131,1.9);
#1274=VECTOR('',#4140,2.);
#1275=VECTOR('',#4143,1.);
#1276=VECTOR('',#4144,1.);
#1277=VECTOR('',#4145,1.);
#1278=VECTOR('',#4146,1.);
#1279=VECTOR('',#4151,1.);
#1280=VECTOR('',#4158,1.);
#1281=VECTOR('',#4163,1.);
#1282=VECTOR('',#4166,1.);
#1283=VECTOR('',#4175,1.);
#1284=VECTOR('',#4194,2.);
#1285=VECTOR('',#4199,1.5);
#1286=VECTOR('',#4206,1.);
#1287=VECTOR('',#4207,1.);
#1288=VECTOR('',#4208,1.);
#1289=VECTOR('',#4209,1.);
#1290=VECTOR('',#4210,1.);
#1291=VECTOR('',#4211,1.);
#1292=VECTOR('',#4216,1.);
#1293=VECTOR('',#4217,1.);
#1294=VECTOR('',#4218,1.);
#1295=VECTOR('',#4221,1.);
#1296=VECTOR('',#4222,1.);
#1297=VECTOR('',#4225,1.);
#1298=VECTOR('',#4226,1.);
#1299=VECTOR('',#4229,1.);
#1300=VECTOR('',#4230,1.);
#1301=VECTOR('',#4233,1.);
#1302=VECTOR('',#4234,1.);
#1303=VECTOR('',#4237,1.);
#1304=VECTOR('',#4242,0.3);
#1305=VECTOR('',#4251,0.4);
#1306=VECTOR('',#4256,0.35);
#1307=VECTOR('',#4267,0.34);
#1308=VECTOR('',#4286,0.5);
#1309=VECTOR('',#4299,0.4);
#1310=VECTOR('',#4304,0.734027674973257);
#1311=VECTOR('',#4311,0.734027674973257);
#1312=VECTOR('',#4314,1.);
#1313=VECTOR('',#4315,1.);
#1314=VECTOR('',#4318,1.);
#1315=VECTOR('',#4321,1.);
#1316=VECTOR('',#4326,0.4);
#1317=VECTOR('',#4329,1.);
#1318=VECTOR('',#4332,1.);
#1319=VECTOR('',#4347,1.);
#1320=VECTOR('',#4352,1.);
#1321=VECTOR('',#4361,1.);
#1322=VECTOR('',#4362,1.);
#1323=VECTOR('',#4363,1.);
#1324=VECTOR('',#4366,1.);
#1325=VECTOR('',#4367,1.);
#1326=VECTOR('',#4368,1.);
#1327=VECTOR('',#4371,1.);
#1328=VECTOR('',#4372,1.);
#1329=VECTOR('',#4373,1.);
#1330=VECTOR('',#4376,1.);
#1331=VECTOR('',#4377,1.);
#1332=VECTOR('',#4378,1.);
#1333=VECTOR('',#4381,1.);
#1334=VECTOR('',#4382,1.);
#1335=VECTOR('',#4389,1.);
#1336=VECTOR('',#4390,1.);
#1337=VECTOR('',#4393,1.);
#1338=VECTOR('',#4394,1.);
#1339=VECTOR('',#4395,1.);
#1340=VECTOR('',#4396,1.);
#1341=VECTOR('',#4399,1.);
#1342=VECTOR('',#4410,1.);
#1343=VECTOR('',#4413,1.);
#1344=VECTOR('',#4416,1.);
#1345=VECTOR('',#4417,1.);
#1346=VECTOR('',#4420,1.);
#1347=VECTOR('',#4421,1.);
#1348=VECTOR('',#4424,1.);
#1349=VECTOR('',#4437,1.);
#1350=VECTOR('',#4438,1.);
#1351=VECTOR('',#4439,1.);
#1352=VECTOR('',#4440,1.);
#1353=VECTOR('',#4441,1.);
#1354=VECTOR('',#4442,1.);
#1355=VECTOR('',#4447,0.425);
#1356=VECTOR('',#4452,0.41);
#1357=VECTOR('',#4461,0.26);
#1358=VECTOR('',#4464,0.25);
#1359=VECTOR('',#4467,1.);
#1360=VECTOR('',#4468,1.);
#1361=VECTOR('',#4469,1.);
#1362=VECTOR('',#4472,1.);
#1363=VECTOR('',#4473,1.);
#1364=VECTOR('',#4476,1.);
#1365=VECTOR('',#4477,1.);
#1366=VECTOR('',#4480,1.);
#1367=VECTOR('',#4481,1.);
#1368=VECTOR('',#4484,1.);
#1369=VECTOR('',#4485,1.);
#1370=VECTOR('',#4488,1.);
#1371=CIRCLE('',#3330,0.275);
#1372=CIRCLE('',#3331,0.275);
#1373=CIRCLE('',#3333,0.275);
#1374=CIRCLE('',#3334,0.275);
#1375=CIRCLE('',#3336,0.34);
#1376=CIRCLE('',#3337,0.34);
#1377=CIRCLE('',#3346,0.5);
#1378=CIRCLE('',#3348,0.5);
#1379=CIRCLE('',#3351,0.5);
#1380=CIRCLE('',#3353,0.5);
#1381=CIRCLE('',#3356,0.5);
#1382=CIRCLE('',#3365,0.21);
#1383=CIRCLE('',#3366,0.21);
#1384=CIRCLE('',#3400,0.21);
#1385=CIRCLE('',#3413,0.5);
#1386=CIRCLE('',#3414,0.5);
#1387=CIRCLE('',#3416,0.5);
#1388=CIRCLE('',#3418,0.5);
#1389=CIRCLE('',#3421,0.275);
#1390=CIRCLE('',#3423,0.275);
#1391=CIRCLE('',#3425,0.3);
#1392=CIRCLE('',#3427,0.3);
#1393=CIRCLE('',#3429,0.275);
#1394=CIRCLE('',#3431,0.275);
#1395=CIRCLE('',#3444,0.425);
#1396=CIRCLE('',#3446,0.24505);
#1397=CIRCLE('',#3448,0.425);
#1398=CIRCLE('',#3450,0.395);
#1399=CIRCLE('',#3452,0.27);
#1400=CIRCLE('',#3454,0.24505);
#1401=CIRCLE('',#3466,1.8);
#1402=CIRCLE('',#3467,2.);
#1403=CIRCLE('',#3470,2.);
#1404=CIRCLE('',#3473,0.5);
#1405=CIRCLE('',#3474,0.5);
#1406=CIRCLE('',#3476,0.5);
#1407=CIRCLE('',#3478,0.5);
#1408=CIRCLE('',#3483,0.48);
#1409=CIRCLE('',#3485,0.332264954516723);
#1410=CIRCLE('',#3487,0.48);
#1411=CIRCLE('',#3488,0.52);
#1412=CIRCLE('',#3490,2.);
#1413=CIRCLE('',#3492,2.);
#1414=CIRCLE('',#3494,1.);
#1415=CIRCLE('',#3498,0.3933);
#1416=CIRCLE('',#3506,0.3);
#1417=CIRCLE('',#3507,0.3);
#1418=CIRCLE('',#3510,0.3933);
#1419=CIRCLE('',#3512,0.3);
#1420=CIRCLE('',#3515,0.5);
#1421=CIRCLE('',#3517,0.34);
#1422=CIRCLE('',#3518,0.34);
#1423=CIRCLE('',#3526,0.5);
#1424=CIRCLE('',#3527,0.5);
#1425=CIRCLE('',#3529,0.338975);
#1426=CIRCLE('',#3531,0.338975);
#1427=CIRCLE('',#3533,0.338975);
#1428=CIRCLE('',#3535,0.6175);
#1429=CIRCLE('',#3537,0.6175);
#1430=CIRCLE('',#3542,0.338975);
#1431=CIRCLE('',#3551,0.5);
#1432=CIRCLE('',#3552,0.5);
#1433=CIRCLE('',#3554,0.5);
#1434=CIRCLE('',#3556,0.5);
#1435=CIRCLE('',#3568,0.2117);
#1436=CIRCLE('',#3569,0.2117);
#1437=CIRCLE('',#3570,0.2117);
#1438=CIRCLE('',#3579,0.425);
#1439=CIRCLE('',#3581,0.24505);
#1440=CIRCLE('',#3583,0.425);
#1441=CIRCLE('',#3585,0.395);
#1442=CIRCLE('',#3587,0.27);
#1443=CIRCLE('',#3589,0.24505);
#1444=VERTEX_POINT('',#4534);
#1445=VERTEX_POINT('',#4536);
#1446=VERTEX_POINT('',#4540);
#1447=VERTEX_POINT('',#4542);
#1448=VERTEX_POINT('',#4546);
#1449=VERTEX_POINT('',#4548);
#1450=VERTEX_POINT('',#4552);
#1451=VERTEX_POINT('',#4553);
#1452=VERTEX_POINT('',#4555);
#1453=VERTEX_POINT('',#4557);
#1454=VERTEX_POINT('',#4561);
#1455=VERTEX_POINT('',#4563);
#1456=VERTEX_POINT('',#4567);
#1457=VERTEX_POINT('',#4569);
#1458=VERTEX_POINT('',#4579);
#1459=VERTEX_POINT('',#4580);
#1460=VERTEX_POINT('',#4582);
#1461=VERTEX_POINT('',#4586);
#1462=VERTEX_POINT('',#4587);
#1463=VERTEX_POINT('',#4589);
#1464=VERTEX_POINT('',#4591);
#1465=VERTEX_POINT('',#4595);
#1466=VERTEX_POINT('',#4596);
#1467=VERTEX_POINT('',#4598);
#1468=VERTEX_POINT('',#4600);
#1469=VERTEX_POINT('',#4602);
#1470=VERTEX_POINT('',#4604);
#1471=VERTEX_POINT('',#4606);
#1472=VERTEX_POINT('',#4614);
#1473=VERTEX_POINT('',#4616);
#1474=VERTEX_POINT('',#4619);
#1475=VERTEX_POINT('',#4623);
#1476=VERTEX_POINT('',#4627);
#1477=VERTEX_POINT('',#4629);
#1478=VERTEX_POINT('',#4633);
#1479=VERTEX_POINT('',#4635);
#1480=VERTEX_POINT('',#4639);
#1481=VERTEX_POINT('',#4641);
#1482=VERTEX_POINT('',#4645);
#1483=VERTEX_POINT('',#4647);
#1484=VERTEX_POINT('',#4649);
#1485=VERTEX_POINT('',#4653);
#1486=VERTEX_POINT('',#4655);
#1487=VERTEX_POINT('',#4659);
#1488=VERTEX_POINT('',#4661);
#1489=VERTEX_POINT('',#4663);
#1490=VERTEX_POINT('',#4665);
#1491=VERTEX_POINT('',#4667);
#1492=VERTEX_POINT('',#4669);
#1493=VERTEX_POINT('',#4671);
#1494=VERTEX_POINT('',#4675);
#1495=VERTEX_POINT('',#4677);
#1496=VERTEX_POINT('',#4679);
#1497=VERTEX_POINT('',#4681);
#1498=VERTEX_POINT('',#4683);
#1499=VERTEX_POINT('',#4685);
#1500=VERTEX_POINT('',#4687);
#1501=VERTEX_POINT('',#4689);
#1502=VERTEX_POINT('',#4691);
#1503=VERTEX_POINT('',#4693);
#1504=VERTEX_POINT('',#4695);
#1505=VERTEX_POINT('',#4697);
#1506=VERTEX_POINT('',#4699);
#1507=VERTEX_POINT('',#4701);
#1508=VERTEX_POINT('',#4703);
#1509=VERTEX_POINT('',#4705);
#1510=VERTEX_POINT('',#4707);
#1511=VERTEX_POINT('',#4709);
#1512=VERTEX_POINT('',#4711);
#1513=VERTEX_POINT('',#4713);
#1514=VERTEX_POINT('',#4715);
#1515=VERTEX_POINT('',#4718);
#1516=VERTEX_POINT('',#4722);
#1517=VERTEX_POINT('',#4723);
#1518=VERTEX_POINT('',#4725);
#1519=VERTEX_POINT('',#4727);
#1520=VERTEX_POINT('',#4731);
#1521=VERTEX_POINT('',#4733);
#1522=VERTEX_POINT('',#4737);
#1523=VERTEX_POINT('',#4739);
#1524=VERTEX_POINT('',#4746);
#1525=VERTEX_POINT('',#4750);
#1526=VERTEX_POINT('',#4754);
#1527=VERTEX_POINT('',#4758);
#1528=VERTEX_POINT('',#4760);
#1529=VERTEX_POINT('',#4764);
#1530=VERTEX_POINT('',#4768);
#1531=VERTEX_POINT('',#4772);
#1532=VERTEX_POINT('',#4776);
#1533=VERTEX_POINT('',#4780);
#1534=VERTEX_POINT('',#4782);
#1535=VERTEX_POINT('',#4786);
#1536=VERTEX_POINT('',#4788);
#1537=VERTEX_POINT('',#4792);
#1538=VERTEX_POINT('',#4794);
#1539=VERTEX_POINT('',#4798);
#1540=VERTEX_POINT('',#4800);
#1541=VERTEX_POINT('',#4804);
#1542=VERTEX_POINT('',#4806);
#1543=VERTEX_POINT('',#4810);
#1544=VERTEX_POINT('',#4814);
#1545=VERTEX_POINT('',#4818);
#1546=VERTEX_POINT('',#4822);
#1547=VERTEX_POINT('',#4826);
#1548=VERTEX_POINT('',#4830);
#1549=VERTEX_POINT('',#4834);
#1550=VERTEX_POINT('',#4838);
#1551=VERTEX_POINT('',#4842);
#1552=VERTEX_POINT('',#4844);
#1553=VERTEX_POINT('',#4848);
#1554=VERTEX_POINT('',#4854);
#1555=VERTEX_POINT('',#4858);
#1556=VERTEX_POINT('',#4862);
#1557=VERTEX_POINT('',#4866);
#1558=VERTEX_POINT('',#4870);
#1559=VERTEX_POINT('',#4874);
#1560=VERTEX_POINT('',#4878);
#1561=VERTEX_POINT('',#4880);
#1562=VERTEX_POINT('',#4887);
#1563=VERTEX_POINT('',#4893);
#1564=VERTEX_POINT('',#4904);
#1565=VERTEX_POINT('',#4905);
#1566=VERTEX_POINT('',#4907);
#1567=VERTEX_POINT('',#4909);
#1568=VERTEX_POINT('',#4911);
#1569=VERTEX_POINT('',#4913);
#1570=VERTEX_POINT('',#4917);
#1571=VERTEX_POINT('',#4919);
#1572=VERTEX_POINT('',#4923);
#1573=VERTEX_POINT('',#4925);
#1574=VERTEX_POINT('',#4929);
#1575=VERTEX_POINT('',#4932);
#1576=VERTEX_POINT('',#4936);
#1577=VERTEX_POINT('',#4938);
#1578=VERTEX_POINT('',#4940);
#1579=VERTEX_POINT('',#4942);
#1580=VERTEX_POINT('',#4944);
#1581=VERTEX_POINT('',#4946);
#1582=VERTEX_POINT('',#4948);
#1583=VERTEX_POINT('',#4950);
#1584=VERTEX_POINT('',#4953);
#1585=VERTEX_POINT('',#4956);
#1586=VERTEX_POINT('',#4958);
#1587=VERTEX_POINT('',#4960);
#1588=VERTEX_POINT('',#4962);
#1589=VERTEX_POINT('',#4964);
#1590=VERTEX_POINT('',#4966);
#1591=VERTEX_POINT('',#4969);
#1592=VERTEX_POINT('',#4972);
#1593=VERTEX_POINT('',#4976);
#1594=VERTEX_POINT('',#4980);
#1595=VERTEX_POINT('',#4984);
#1596=VERTEX_POINT('',#4988);
#1597=VERTEX_POINT('',#4990);
#1598=VERTEX_POINT('',#4996);
#1599=VERTEX_POINT('',#4998);
#1600=VERTEX_POINT('',#5000);
#1601=VERTEX_POINT('',#5002);
#1602=VERTEX_POINT('',#5010);
#1603=VERTEX_POINT('',#5015);
#1604=VERTEX_POINT('',#5025);
#1605=VERTEX_POINT('',#5028);
#1606=VERTEX_POINT('',#5030);
#1607=VERTEX_POINT('',#5031);
#1608=VERTEX_POINT('',#5033);
#1609=VERTEX_POINT('',#5035);
#1610=VERTEX_POINT('',#5037);
#1611=VERTEX_POINT('',#5039);
#1612=VERTEX_POINT('',#5043);
#1613=VERTEX_POINT('',#5047);
#1614=VERTEX_POINT('',#5051);
#1615=VERTEX_POINT('',#5054);
#1616=VERTEX_POINT('',#5060);
#1617=VERTEX_POINT('',#5061);
#1618=VERTEX_POINT('',#5066);
#1619=VERTEX_POINT('',#5070);
#1620=VERTEX_POINT('',#5074);
#1621=VERTEX_POINT('',#5078);
#1622=VERTEX_POINT('',#5087);
#1623=VERTEX_POINT('',#5089);
#1624=VERTEX_POINT('',#5094);
#1625=VERTEX_POINT('',#5098);
#1626=VERTEX_POINT('',#5099);
#1627=VERTEX_POINT('',#5101);
#1628=VERTEX_POINT('',#5103);
#1629=VERTEX_POINT('',#5107);
#1630=VERTEX_POINT('',#5109);
#1631=VERTEX_POINT('',#5113);
#1632=VERTEX_POINT('',#5117);
#1633=VERTEX_POINT('',#5125);
#1634=VERTEX_POINT('',#5126);
#1635=VERTEX_POINT('',#5132);
#1636=VERTEX_POINT('',#5134);
#1637=VERTEX_POINT('',#5137);
#1638=VERTEX_POINT('',#5140);
#1639=VERTEX_POINT('',#5144);
#1640=VERTEX_POINT('',#5150);
#1641=VERTEX_POINT('',#5151);
#1642=VERTEX_POINT('',#5153);
#1643=VERTEX_POINT('',#5155);
#1644=VERTEX_POINT('',#5157);
#1645=VERTEX_POINT('',#5159);
#1646=VERTEX_POINT('',#5162);
#1647=VERTEX_POINT('',#5165);
#1648=VERTEX_POINT('',#5166);
#1649=VERTEX_POINT('',#5171);
#1650=VERTEX_POINT('',#5175);
#1651=VERTEX_POINT('',#5179);
#1652=VERTEX_POINT('',#5183);
#1653=VERTEX_POINT('',#5189);
#1654=VERTEX_POINT('',#5191);
#1655=VERTEX_POINT('',#5196);
#1656=VERTEX_POINT('',#5200);
#1657=VERTEX_POINT('',#5205);
#1658=VERTEX_POINT('',#5208);
#1659=VERTEX_POINT('',#5210);
#1660=VERTEX_POINT('',#5220);
#1661=VERTEX_POINT('',#5222);
#1662=VERTEX_POINT('',#5226);
#1663=VERTEX_POINT('',#5229);
#1664=VERTEX_POINT('',#5232);
#1665=VERTEX_POINT('',#5236);
#1666=VERTEX_POINT('',#5237);
#1667=VERTEX_POINT('',#5241);
#1668=VERTEX_POINT('',#5245);
#1669=VERTEX_POINT('',#5248);
#1670=VERTEX_POINT('',#5252);
#1671=VERTEX_POINT('',#5256);
#1672=VERTEX_POINT('',#5264);
#1673=VERTEX_POINT('',#5266);
#1674=VERTEX_POINT('',#5268);
#1675=VERTEX_POINT('',#5272);
#1676=VERTEX_POINT('',#5276);
#1677=VERTEX_POINT('',#5280);
#1678=VERTEX_POINT('',#5284);
#1679=VERTEX_POINT('',#5299);
#1680=VERTEX_POINT('',#5311);
#1681=VERTEX_POINT('',#5312);
#1682=VERTEX_POINT('',#5314);
#1683=VERTEX_POINT('',#5316);
#1684=VERTEX_POINT('',#5320);
#1685=VERTEX_POINT('',#5321);
#1686=VERTEX_POINT('',#5323);
#1687=VERTEX_POINT('',#5325);
#1688=VERTEX_POINT('',#5329);
#1689=VERTEX_POINT('',#5331);
#1690=VERTEX_POINT('',#5335);
#1691=VERTEX_POINT('',#5337);
#1692=VERTEX_POINT('',#5341);
#1693=VERTEX_POINT('',#5343);
#1694=VERTEX_POINT('',#5347);
#1695=VERTEX_POINT('',#5349);
#1696=VERTEX_POINT('',#5353);
#1697=VERTEX_POINT('',#5355);
#1698=VERTEX_POINT('',#5359);
#1699=VERTEX_POINT('',#5361);
#1700=VERTEX_POINT('',#5365);
#1701=VERTEX_POINT('',#5366);
#1702=VERTEX_POINT('',#5368);
#1703=VERTEX_POINT('',#5370);
#1704=VERTEX_POINT('',#5372);
#1705=VERTEX_POINT('',#5374);
#1706=VERTEX_POINT('',#5386);
#1707=VERTEX_POINT('',#5390);
#1708=VERTEX_POINT('',#5398);
#1709=VERTEX_POINT('',#5401);
#1710=VERTEX_POINT('',#5403);
#1711=VERTEX_POINT('',#5404);
#1712=VERTEX_POINT('',#5406);
#1713=VERTEX_POINT('',#5408);
#1714=VERTEX_POINT('',#5410);
#1715=VERTEX_POINT('',#5412);
#1716=VERTEX_POINT('',#5416);
#1717=VERTEX_POINT('',#5420);
#1718=VERTEX_POINT('',#5424);
#1719=VERTEX_POINT('',#5427);
#1720=VERTEX_POINT('',#5433);
#1721=VERTEX_POINT('',#5434);
#1722=VERTEX_POINT('',#5439);
#1723=VERTEX_POINT('',#5443);
#1724=VERTEX_POINT('',#5447);
#1725=VERTEX_POINT('',#5451);
#1726=EDGE_CURVE('',#1444,#1444,#1371,.T.);
#1727=EDGE_CURVE('',#1444,#1445,#709,.T.);
#1728=EDGE_CURVE('',#1445,#1445,#1372,.T.);
#1729=EDGE_CURVE('',#1446,#1446,#1373,.T.);
#1730=EDGE_CURVE('',#1446,#1447,#710,.T.);
#1731=EDGE_CURVE('',#1447,#1447,#1374,.T.);
#1732=EDGE_CURVE('',#1448,#1448,#1375,.T.);
#1733=EDGE_CURVE('',#1448,#1449,#711,.T.);
#1734=EDGE_CURVE('',#1449,#1449,#1376,.T.);
#1735=EDGE_CURVE('',#1450,#1451,#712,.T.);
#1736=EDGE_CURVE('',#1451,#1452,#713,.T.);
#1737=EDGE_CURVE('',#1453,#1452,#714,.T.);
#1738=EDGE_CURVE('',#1450,#1453,#715,.T.);
#1739=EDGE_CURVE('',#1454,#1450,#716,.T.);
#1740=EDGE_CURVE('',#1455,#1453,#717,.T.);
#1741=EDGE_CURVE('',#1454,#1455,#718,.T.);
#1742=EDGE_CURVE('',#1456,#1454,#719,.T.);
#1743=EDGE_CURVE('',#1457,#1455,#720,.T.);
#1744=EDGE_CURVE('',#1456,#1457,#721,.T.);
#1745=EDGE_CURVE('',#1451,#1456,#722,.T.);
#1746=EDGE_CURVE('',#1452,#1457,#723,.T.);
#1747=EDGE_CURVE('',#1458,#1459,#724,.T.);
#1748=EDGE_CURVE('',#1460,#1458,#1377,.T.);
#1749=EDGE_CURVE('',#1459,#1460,#725,.T.);
#1750=EDGE_CURVE('',#1461,#1462,#726,.T.);
#1751=EDGE_CURVE('',#1461,#1463,#1378,.T.);
#1752=EDGE_CURVE('',#1464,#1463,#727,.T.);
#1753=EDGE_CURVE('',#1462,#1464,#728,.T.);
#1754=EDGE_CURVE('',#1465,#1466,#129,.T.);
#1755=EDGE_CURVE('',#1465,#1467,#1379,.T.);
#1756=EDGE_CURVE('',#1468,#1467,#729,.T.);
#1757=EDGE_CURVE('',#1469,#1468,#130,.T.);
#1758=EDGE_CURVE('',#1470,#1469,#730,.T.);
#1759=EDGE_CURVE('',#1471,#1470,#1380,.T.);
#1760=EDGE_CURVE('',#1463,#1471,#128,.T.);
#1761=EDGE_CURVE('',#1472,#1461,#731,.T.);
#1762=EDGE_CURVE('',#1473,#1472,#131,.T.);
#1763=EDGE_CURVE('',#1460,#1473,#732,.T.);
#1764=EDGE_CURVE('',#1474,#1458,#132,.T.);
#1765=EDGE_CURVE('',#1466,#1474,#1381,.T.);
#1766=EDGE_CURVE('',#1475,#1465,#733,.T.);
#1767=EDGE_CURVE('',#1467,#1475,#734,.T.);
#1768=EDGE_CURVE('',#1476,#1470,#735,.T.);
#1769=EDGE_CURVE('',#1477,#1476,#736,.T.);
#1770=EDGE_CURVE('',#1471,#1477,#737,.T.);
#1771=EDGE_CURVE('',#1474,#1478,#738,.T.);
#1772=EDGE_CURVE('',#1479,#1478,#739,.T.);
#1773=EDGE_CURVE('',#1466,#1479,#740,.T.);
#1774=EDGE_CURVE('',#1480,#1459,#741,.T.);
#1775=EDGE_CURVE('',#1480,#1481,#742,.T.);
#1776=EDGE_CURVE('',#1478,#1481,#743,.T.);
#1777=EDGE_CURVE('',#1472,#1482,#744,.T.);
#1778=EDGE_CURVE('',#1483,#1482,#745,.T.);
#1779=EDGE_CURVE('',#1484,#1483,#746,.T.);
#1780=EDGE_CURVE('',#1473,#1484,#747,.T.);
#1781=EDGE_CURVE('',#1485,#1462,#748,.T.);
#1782=EDGE_CURVE('',#1485,#1486,#749,.T.);
#1783=EDGE_CURVE('',#1482,#1486,#750,.T.);
#1784=EDGE_CURVE('',#1484,#1487,#751,.T.);
#1785=EDGE_CURVE('',#1487,#1488,#752,.T.);
#1786=EDGE_CURVE('',#1488,#1489,#753,.T.);
#1787=EDGE_CURVE('',#1490,#1489,#754,.T.);
#1788=EDGE_CURVE('',#1491,#1490,#755,.T.);
#1789=EDGE_CURVE('',#1491,#1492,#756,.T.);
#1790=EDGE_CURVE('',#1492,#1493,#757,.T.);
#1791=EDGE_CURVE('',#1493,#1480,#758,.T.);
#1792=EDGE_CURVE('',#1476,#1494,#759,.T.);
#1793=EDGE_CURVE('',#1494,#1495,#760,.T.);
#1794=EDGE_CURVE('',#1495,#1496,#761,.T.);
#1795=EDGE_CURVE('',#1496,#1497,#762,.T.);
#1796=EDGE_CURVE('',#1497,#1498,#763,.T.);
#1797=EDGE_CURVE('',#1499,#1498,#764,.T.);
#1798=EDGE_CURVE('',#1500,#1499,#765,.T.);
#1799=EDGE_CURVE('',#1500,#1501,#766,.T.);
#1800=EDGE_CURVE('',#1501,#1502,#767,.T.);
#1801=EDGE_CURVE('',#1502,#1503,#768,.T.);
#1802=EDGE_CURVE('',#1503,#1504,#769,.T.);
#1803=EDGE_CURVE('',#1504,#1505,#770,.T.);
#1804=EDGE_CURVE('',#1505,#1506,#771,.T.);
#1805=EDGE_CURVE('',#1506,#1507,#772,.T.);
#1806=EDGE_CURVE('',#1507,#1508,#773,.T.);
#1807=EDGE_CURVE('',#1508,#1509,#774,.T.);
#1808=EDGE_CURVE('',#1510,#1509,#775,.T.);
#1809=EDGE_CURVE('',#1511,#1510,#776,.T.);
#1810=EDGE_CURVE('',#1511,#1512,#777,.T.);
#1811=EDGE_CURVE('',#1512,#1513,#778,.T.);
#1812=EDGE_CURVE('',#1513,#1514,#779,.T.);
#1813=EDGE_CURVE('',#1514,#1485,#780,.T.);
#1814=EDGE_CURVE('',#1464,#1515,#1382,.T.);
#1815=EDGE_CURVE('',#1515,#1477,#1383,.T.);
#1816=EDGE_CURVE('',#1516,#1517,#781,.T.);
#1817=EDGE_CURVE('',#1516,#1518,#782,.T.);
#1818=EDGE_CURVE('',#1519,#1518,#783,.T.);
#1819=EDGE_CURVE('',#1517,#1519,#784,.T.);
#1820=EDGE_CURVE('',#1520,#1516,#785,.T.);
#1821=EDGE_CURVE('',#1520,#1521,#786,.T.);
#1822=EDGE_CURVE('',#1518,#1521,#787,.T.);
#1823=EDGE_CURVE('',#1522,#1520,#788,.T.);
#1824=EDGE_CURVE('',#1522,#1523,#789,.T.);
#1825=EDGE_CURVE('',#1521,#1523,#790,.T.);
#1826=EDGE_CURVE('',#1523,#1479,#791,.T.);
#1827=EDGE_CURVE('',#1475,#1522,#792,.T.);
#1828=EDGE_CURVE('',#1493,#1524,#793,.T.);
#1829=EDGE_CURVE('',#1481,#1524,#794,.T.);
#1830=EDGE_CURVE('',#1492,#1525,#795,.T.);
#1831=EDGE_CURVE('',#1524,#1525,#796,.T.);
#1832=EDGE_CURVE('',#1526,#1491,#797,.T.);
#1833=EDGE_CURVE('',#1525,#1526,#798,.T.);
#1834=EDGE_CURVE('',#1497,#1527,#799,.T.);
#1835=EDGE_CURVE('',#1528,#1527,#800,.T.);
#1836=EDGE_CURVE('',#1498,#1528,#801,.T.);
#1837=EDGE_CURVE('',#1496,#1529,#802,.T.);
#1838=EDGE_CURVE('',#1527,#1529,#803,.T.);
#1839=EDGE_CURVE('',#1495,#1530,#804,.T.);
#1840=EDGE_CURVE('',#1529,#1530,#805,.T.);
#1841=EDGE_CURVE('',#1494,#1531,#806,.T.);
#1842=EDGE_CURVE('',#1530,#1531,#807,.T.);
#1843=EDGE_CURVE('',#1469,#1532,#808,.T.);
#1844=EDGE_CURVE('',#1531,#1532,#809,.T.);
#1845=EDGE_CURVE('',#1533,#1468,#810,.T.);
#1846=EDGE_CURVE('',#1533,#1534,#811,.T.);
#1847=EDGE_CURVE('',#1532,#1534,#812,.T.);
#1848=EDGE_CURVE('',#1535,#1533,#813,.T.);
#1849=EDGE_CURVE('',#1535,#1536,#814,.T.);
#1850=EDGE_CURVE('',#1534,#1536,#815,.T.);
#1851=EDGE_CURVE('',#1537,#1535,#816,.T.);
#1852=EDGE_CURVE('',#1537,#1538,#817,.T.);
#1853=EDGE_CURVE('',#1536,#1538,#818,.T.);
#1854=EDGE_CURVE('',#1539,#1537,#819,.T.);
#1855=EDGE_CURVE('',#1540,#1539,#820,.T.);
#1856=EDGE_CURVE('',#1538,#1540,#821,.T.);
#1857=EDGE_CURVE('',#1508,#1541,#822,.T.);
#1858=EDGE_CURVE('',#1542,#1541,#823,.T.);
#1859=EDGE_CURVE('',#1509,#1542,#824,.T.);
#1860=EDGE_CURVE('',#1507,#1543,#825,.T.);
#1861=EDGE_CURVE('',#1541,#1543,#826,.T.);
#1862=EDGE_CURVE('',#1506,#1544,#827,.T.);
#1863=EDGE_CURVE('',#1543,#1544,#828,.T.);
#1864=EDGE_CURVE('',#1505,#1545,#829,.T.);
#1865=EDGE_CURVE('',#1544,#1545,#830,.T.);
#1866=EDGE_CURVE('',#1504,#1546,#831,.T.);
#1867=EDGE_CURVE('',#1545,#1546,#832,.T.);
#1868=EDGE_CURVE('',#1503,#1547,#833,.T.);
#1869=EDGE_CURVE('',#1546,#1547,#834,.T.);
#1870=EDGE_CURVE('',#1502,#1548,#835,.T.);
#1871=EDGE_CURVE('',#1547,#1548,#836,.T.);
#1872=EDGE_CURVE('',#1501,#1549,#837,.T.);
#1873=EDGE_CURVE('',#1548,#1549,#838,.T.);
#1874=EDGE_CURVE('',#1550,#1500,#839,.T.);
#1875=EDGE_CURVE('',#1549,#1550,#840,.T.);
#1876=EDGE_CURVE('',#1488,#1551,#841,.T.);
#1877=EDGE_CURVE('',#1552,#1551,#842,.T.);
#1878=EDGE_CURVE('',#1489,#1552,#843,.T.);
#1879=EDGE_CURVE('',#1487,#1553,#844,.T.);
#1880=EDGE_CURVE('',#1551,#1553,#845,.T.);
#1881=EDGE_CURVE('',#1553,#1483,#846,.T.);
#1882=EDGE_CURVE('',#1514,#1554,#847,.T.);
#1883=EDGE_CURVE('',#1486,#1554,#848,.T.);
#1884=EDGE_CURVE('',#1513,#1555,#849,.T.);
#1885=EDGE_CURVE('',#1554,#1555,#850,.T.);
#1886=EDGE_CURVE('',#1512,#1556,#851,.T.);
#1887=EDGE_CURVE('',#1555,#1556,#852,.T.);
#1888=EDGE_CURVE('',#1557,#1511,#853,.T.);
#1889=EDGE_CURVE('',#1556,#1557,#854,.T.);
#1890=EDGE_CURVE('',#1515,#1558,#855,.T.);
#1891=EDGE_CURVE('',#1558,#1558,#1384,.T.);
#1892=EDGE_CURVE('',#1490,#1559,#856,.T.);
#1893=EDGE_CURVE('',#1526,#1559,#857,.T.);
#1894=EDGE_CURVE('',#1560,#1519,#858,.T.);
#1895=EDGE_CURVE('',#1561,#1560,#859,.T.);
#1896=EDGE_CURVE('',#1561,#1517,#860,.T.);
#1897=EDGE_CURVE('',#1539,#1561,#861,.T.);
#1898=EDGE_CURVE('',#1540,#1560,#862,.T.);
#1899=EDGE_CURVE('',#1562,#1528,#863,.T.);
#1900=EDGE_CURVE('',#1499,#1562,#864,.T.);
#1901=EDGE_CURVE('',#1550,#1562,#865,.T.);
#1902=EDGE_CURVE('',#1563,#1542,#866,.T.);
#1903=EDGE_CURVE('',#1510,#1563,#867,.T.);
#1904=EDGE_CURVE('',#1557,#1563,#868,.T.);
#1905=EDGE_CURVE('',#1559,#1552,#869,.T.);
#1906=EDGE_CURVE('',#1564,#1565,#870,.T.);
#1907=EDGE_CURVE('',#1564,#1566,#1385,.T.);
#1908=EDGE_CURVE('',#1567,#1566,#871,.T.);
#1909=EDGE_CURVE('',#1568,#1567,#872,.T.);
#1910=EDGE_CURVE('',#1568,#1569,#1386,.T.);
#1911=EDGE_CURVE('',#1565,#1569,#873,.T.);
#1912=EDGE_CURVE('',#1569,#1570,#874,.T.);
#1913=EDGE_CURVE('',#1571,#1568,#875,.T.);
#1914=EDGE_CURVE('',#1571,#1570,#1387,.T.);
#1915=EDGE_CURVE('',#1572,#1564,#876,.T.);
#1916=EDGE_CURVE('',#1572,#1573,#1388,.T.);
#1917=EDGE_CURVE('',#1566,#1573,#877,.T.);
#1918=EDGE_CURVE('',#1574,#1572,#878,.T.);
#1919=EDGE_CURVE('',#1570,#1574,#879,.T.);
#1920=EDGE_CURVE('',#1575,#1571,#880,.T.);
#1921=EDGE_CURVE('',#1573,#1575,#881,.T.);
#1922=EDGE_CURVE('',#1576,#1565,#882,.T.);
#1923=EDGE_CURVE('',#1576,#1577,#883,.T.);
#1924=EDGE_CURVE('',#1577,#1578,#884,.T.);
#1925=EDGE_CURVE('',#1579,#1578,#885,.T.);
#1926=EDGE_CURVE('',#1579,#1580,#886,.T.);
#1927=EDGE_CURVE('',#1581,#1580,#887,.T.);
#1928=EDGE_CURVE('',#1581,#1582,#888,.T.);
#1929=EDGE_CURVE('',#1582,#1583,#889,.T.);
#1930=EDGE_CURVE('',#1574,#1583,#890,.T.);
#1931=EDGE_CURVE('',#1584,#1584,#1389,.T.);
#1932=EDGE_CURVE('',#1585,#1567,#891,.T.);
#1933=EDGE_CURVE('',#1585,#1586,#892,.T.);
#1934=EDGE_CURVE('',#1586,#1587,#893,.T.);
#1935=EDGE_CURVE('',#1588,#1587,#894,.T.);
#1936=EDGE_CURVE('',#1589,#1588,#895,.T.);
#1937=EDGE_CURVE('',#1590,#1589,#896,.T.);
#1938=EDGE_CURVE('',#1575,#1590,#897,.T.);
#1939=EDGE_CURVE('',#1591,#1591,#1390,.T.);
#1940=EDGE_CURVE('',#1592,#1585,#898,.T.);
#1941=EDGE_CURVE('',#1586,#1592,#1391,.T.);
#1942=EDGE_CURVE('',#1593,#1592,#899,.T.);
#1943=EDGE_CURVE('',#1587,#1593,#1392,.T.);
#1944=EDGE_CURVE('',#1591,#1594,#900,.T.);
#1945=EDGE_CURVE('',#1594,#1594,#1393,.T.);
#1946=EDGE_CURVE('',#1595,#1595,#1394,.T.);
#1947=EDGE_CURVE('',#1595,#1584,#901,.T.);
#1948=EDGE_CURVE('',#1596,#1581,#902,.T.);
#1949=EDGE_CURVE('',#1597,#1596,#903,.T.);
#1950=EDGE_CURVE('',#1582,#1597,#904,.T.);
#1951=EDGE_CURVE('',#1583,#1597,#905,.T.);
#1952=EDGE_CURVE('',#1598,#1596,#906,.T.);
#1953=EDGE_CURVE('',#1599,#1598,#907,.T.);
#1954=EDGE_CURVE('',#1600,#1599,#908,.T.);
#1955=EDGE_CURVE('',#1600,#1601,#909,.T.);
#1956=EDGE_CURVE('',#1601,#1576,#910,.T.);
#1957=EDGE_CURVE('',#1578,#1600,#911,.T.);
#1958=EDGE_CURVE('',#1577,#1601,#912,.T.);
#1959=EDGE_CURVE('',#1593,#1602,#913,.T.);
#1960=EDGE_CURVE('',#1602,#1579,#914,.T.);
#1961=EDGE_CURVE('',#1599,#1588,#915,.T.);
#1962=EDGE_CURVE('',#1603,#1590,#916,.T.);
#1963=EDGE_CURVE('',#1602,#1603,#917,.T.);
#1964=EDGE_CURVE('',#1580,#1603,#918,.T.);
#1965=EDGE_CURVE('',#1589,#1598,#919,.T.);
#1966=EDGE_CURVE('',#1604,#1604,#1395,.T.);
#1967=EDGE_CURVE('',#1605,#1605,#1396,.T.);
#1968=EDGE_CURVE('',#1606,#1607,#920,.T.);
#1969=EDGE_CURVE('',#1608,#1606,#921,.T.);
#1970=EDGE_CURVE('',#1609,#1608,#922,.T.);
#1971=EDGE_CURVE('',#1610,#1609,#923,.T.);
#1972=EDGE_CURVE('',#1611,#1610,#924,.T.);
#1973=EDGE_CURVE('',#1607,#1611,#925,.T.);
#1974=EDGE_CURVE('',#1612,#1612,#1397,.T.);
#1975=EDGE_CURVE('',#1612,#1604,#926,.T.);
#1976=EDGE_CURVE('',#1613,#1613,#1398,.T.);
#1977=EDGE_CURVE('',#1613,#1612,#927,.T.);
#1978=EDGE_CURVE('',#1614,#1614,#1399,.T.);
#1979=EDGE_CURVE('',#1615,#1615,#1400,.F.);
#1980=EDGE_CURVE('',#1615,#1614,#928,.T.);
#1981=EDGE_CURVE('',#1605,#1615,#929,.T.);
#1982=EDGE_CURVE('',#1616,#1617,#930,.T.);
#1983=EDGE_CURVE('',#1617,#1606,#931,.T.);
#1984=EDGE_CURVE('',#1616,#1607,#932,.T.);
#1985=EDGE_CURVE('',#1617,#1618,#933,.T.);
#1986=EDGE_CURVE('',#1618,#1608,#934,.T.);
#1987=EDGE_CURVE('',#1618,#1619,#935,.T.);
#1988=EDGE_CURVE('',#1619,#1609,#936,.T.);
#1989=EDGE_CURVE('',#1619,#1620,#937,.T.);
#1990=EDGE_CURVE('',#1620,#1610,#938,.T.);
#1991=EDGE_CURVE('',#1620,#1621,#939,.T.);
#1992=EDGE_CURVE('',#1621,#1611,#940,.T.);
#1993=EDGE_CURVE('',#1621,#1616,#941,.T.);
#1994=EDGE_CURVE('',#1622,#1622,#1401,.T.);
#1995=EDGE_CURVE('',#1622,#1623,#942,.T.);
#1996=EDGE_CURVE('',#1623,#1623,#1402,.T.);
#1997=EDGE_CURVE('',#1624,#1624,#1403,.T.);
#1998=EDGE_CURVE('',#1624,#1623,#943,.T.);
#1999=EDGE_CURVE('',#1625,#1626,#944,.T.);
#2000=EDGE_CURVE('',#1627,#1625,#945,.T.);
#2001=EDGE_CURVE('',#1628,#1627,#946,.T.);
#2002=EDGE_CURVE('',#1626,#1628,#947,.T.);
#2003=EDGE_CURVE('',#1627,#1629,#1404,.T.);
#2004=EDGE_CURVE('',#1630,#1629,#948,.T.);
#2005=EDGE_CURVE('',#1630,#1628,#1405,.T.);
#2006=EDGE_CURVE('',#1625,#1631,#1406,.T.);
#2007=EDGE_CURVE('',#1629,#1631,#949,.T.);
#2008=EDGE_CURVE('',#1632,#1626,#1407,.T.);
#2009=EDGE_CURVE('',#1631,#1632,#950,.T.);
#2010=EDGE_CURVE('',#1632,#1630,#951,.T.);
#2011=EDGE_CURVE('',#1633,#1634,#1408,.T.);
#2012=EDGE_CURVE('',#1634,#1633,#952,.T.);
#2013=EDGE_CURVE('',#1634,#1633,#1409,.T.);
#2014=EDGE_CURVE('',#1635,#1635,#1410,.T.);
#2015=EDGE_CURVE('',#1636,#1635,#1411,.T.);
#2016=EDGE_CURVE('',#1637,#1637,#1412,.T.);
#2017=EDGE_CURVE('',#1638,#1638,#1413,.T.);
#2018=EDGE_CURVE('',#1638,#1637,#953,.T.);
#2019=EDGE_CURVE('',#1639,#1639,#1414,.T.);
#2020=EDGE_CURVE('',#1639,#1638,#954,.T.);
#2021=EDGE_CURVE('',#1640,#1641,#955,.T.);
#2022=EDGE_CURVE('',#1641,#1642,#956,.T.);
#2023=EDGE_CURVE('',#1642,#1643,#957,.T.);
#2024=EDGE_CURVE('',#1643,#1644,#958,.T.);
#2025=EDGE_CURVE('',#1644,#1645,#959,.T.);
#2026=EDGE_CURVE('',#1645,#1640,#960,.T.);
#2027=EDGE_CURVE('',#1646,#1646,#1415,.F.);
#2028=EDGE_CURVE('',#1647,#1648,#961,.T.);
#2029=EDGE_CURVE('',#1648,#1640,#962,.T.);
#2030=EDGE_CURVE('',#1647,#1645,#963,.T.);
#2031=EDGE_CURVE('',#1649,#1647,#964,.T.);
#2032=EDGE_CURVE('',#1649,#1644,#965,.T.);
#2033=EDGE_CURVE('',#1650,#1649,#966,.T.);
#2034=EDGE_CURVE('',#1650,#1643,#967,.T.);
#2035=EDGE_CURVE('',#1651,#1650,#968,.T.);
#2036=EDGE_CURVE('',#1651,#1642,#969,.T.);
#2037=EDGE_CURVE('',#1652,#1651,#970,.T.);
#2038=EDGE_CURVE('',#1652,#1641,#971,.T.);
#2039=EDGE_CURVE('',#1648,#1652,#972,.T.);
#2040=EDGE_CURVE('',#1653,#1653,#1416,.T.);
#2041=EDGE_CURVE('',#1653,#1654,#973,.T.);
#2042=EDGE_CURVE('',#1654,#1654,#1417,.T.);
#2043=EDGE_CURVE('',#1655,#1655,#1418,.F.);
#2044=EDGE_CURVE('',#1655,#1646,#974,.T.);
#2045=EDGE_CURVE('',#1656,#1656,#1419,.T.);
#2046=EDGE_CURVE('',#1656,#1655,#975,.T.);
#2047=EDGE_CURVE('',#1654,#1657,#1420,.T.);
#2048=EDGE_CURVE('',#1658,#1658,#1421,.T.);
#2049=EDGE_CURVE('',#1658,#1659,#976,.T.);
#2050=EDGE_CURVE('',#1659,#1659,#1422,.T.);
#2051=EDGE_CURVE('',#1660,#1660,#1423,.T.);
#2052=EDGE_CURVE('',#1660,#1661,#977,.T.);
#2053=EDGE_CURVE('',#1661,#1661,#1424,.T.);
#2054=EDGE_CURVE('',#1662,#1662,#1425,.T.);
#2055=EDGE_CURVE('',#1663,#1663,#1426,.T.);
#2056=EDGE_CURVE('',#1663,#1664,#978,.T.);
#2057=EDGE_CURVE('',#1664,#1664,#1427,.F.);
#2058=EDGE_CURVE('',#1665,#1666,#11,.T.);
#2059=EDGE_CURVE('',#1667,#1665,#12,.T.);
#2060=EDGE_CURVE('',#1667,#1668,#979,.T.);
#2061=EDGE_CURVE('',#1668,#1668,#1428,.T.);
#2062=EDGE_CURVE('',#1669,#1667,#13,.T.);
#2063=EDGE_CURVE('',#1670,#1669,#14,.T.);
#2064=EDGE_CURVE('',#1671,#1670,#15,.T.);
#2065=EDGE_CURVE('',#1666,#1671,#16,.T.);
#2066=EDGE_CURVE('',#1672,#1672,#1429,.T.);
#2067=EDGE_CURVE('',#1672,#1673,#980,.T.);
#2068=EDGE_CURVE('',#1674,#1673,#17,.T.);
#2069=EDGE_CURVE('',#1675,#1674,#18,.T.);
#2070=EDGE_CURVE('',#1676,#1675,#19,.T.);
#2071=EDGE_CURVE('',#1677,#1676,#20,.T.);
#2072=EDGE_CURVE('',#1678,#1677,#21,.T.);
#2073=EDGE_CURVE('',#1673,#1678,#22,.T.);
#2074=EDGE_CURVE('',#1669,#1678,#981,.T.);
#2075=EDGE_CURVE('',#1670,#1677,#982,.T.);
#2076=EDGE_CURVE('',#1667,#1673,#983,.T.);
#2077=EDGE_CURVE('',#1665,#1674,#984,.T.);
#2078=EDGE_CURVE('',#1679,#1679,#1430,.F.);
#2079=EDGE_CURVE('',#1679,#1662,#985,.T.);
#2080=EDGE_CURVE('',#1666,#1675,#986,.T.);
#2081=EDGE_CURVE('',#1671,#1676,#987,.T.);
#2082=EDGE_CURVE('',#1680,#1681,#133,.T.);
#2083=EDGE_CURVE('',#1682,#1680,#1431,.T.);
#2084=EDGE_CURVE('',#1683,#1682,#988,.T.);
#2085=EDGE_CURVE('',#1681,#1683,#1432,.T.);
#2086=EDGE_CURVE('',#1684,#1685,#989,.T.);
#2087=EDGE_CURVE('',#1686,#1684,#1433,.T.);
#2088=EDGE_CURVE('',#1687,#1686,#134,.T.);
#2089=EDGE_CURVE('',#1685,#1687,#1434,.T.);
#2090=EDGE_CURVE('',#1688,#1680,#990,.T.);
#2091=EDGE_CURVE('',#1689,#1688,#991,.T.);
#2092=EDGE_CURVE('',#1682,#1689,#992,.T.);
#2093=EDGE_CURVE('',#1690,#1684,#993,.T.);
#2094=EDGE_CURVE('',#1691,#1690,#994,.T.);
#2095=EDGE_CURVE('',#1686,#1691,#995,.T.);
#2096=EDGE_CURVE('',#1692,#1683,#996,.T.);
#2097=EDGE_CURVE('',#1693,#1692,#997,.T.);
#2098=EDGE_CURVE('',#1681,#1693,#998,.T.);
#2099=EDGE_CURVE('',#1694,#1687,#999,.T.);
#2100=EDGE_CURVE('',#1694,#1695,#1000,.T.);
#2101=EDGE_CURVE('',#1685,#1695,#1001,.T.);
#2102=EDGE_CURVE('',#1693,#1696,#1002,.T.);
#2103=EDGE_CURVE('',#1696,#1697,#1003,.T.);
#2104=EDGE_CURVE('',#1697,#1688,#135,.T.);
#2105=EDGE_CURVE('',#1691,#1698,#136,.T.);
#2106=EDGE_CURVE('',#1698,#1699,#1004,.T.);
#2107=EDGE_CURVE('',#1699,#1694,#1005,.T.);
#2108=EDGE_CURVE('',#1700,#1701,#1006,.T.);
#2109=EDGE_CURVE('',#1701,#1702,#1007,.T.);
#2110=EDGE_CURVE('',#1702,#1703,#1008,.T.);
#2111=EDGE_CURVE('',#1703,#1704,#1009,.T.);
#2112=EDGE_CURVE('',#1704,#1705,#137,.T.);
#2113=EDGE_CURVE('',#1705,#1700,#1010,.T.);
#2114=EDGE_CURVE('',#1689,#1690,#1435,.T.);
#2115=EDGE_CURVE('',#1705,#1697,#1436,.F.);
#2116=EDGE_CURVE('',#1698,#1704,#1437,.F.);
#2117=EDGE_CURVE('',#1699,#1703,#1011,.T.);
#2118=EDGE_CURVE('',#1700,#1696,#1012,.T.);
#2119=EDGE_CURVE('',#1706,#1692,#1013,.T.);
#2120=EDGE_CURVE('',#1701,#1706,#1014,.T.);
#2121=EDGE_CURVE('',#1707,#1706,#1015,.T.);
#2122=EDGE_CURVE('',#1702,#1707,#1016,.T.);
#2123=EDGE_CURVE('',#1695,#1707,#1017,.T.);
#2124=EDGE_CURVE('',#1708,#1708,#1438,.T.);
#2125=EDGE_CURVE('',#1709,#1709,#1439,.T.);
#2126=EDGE_CURVE('',#1710,#1711,#1018,.T.);
#2127=EDGE_CURVE('',#1712,#1710,#1019,.T.);
#2128=EDGE_CURVE('',#1713,#1712,#1020,.T.);
#2129=EDGE_CURVE('',#1714,#1713,#1021,.T.);
#2130=EDGE_CURVE('',#1715,#1714,#1022,.T.);
#2131=EDGE_CURVE('',#1711,#1715,#1023,.T.);
#2132=EDGE_CURVE('',#1716,#1716,#1440,.T.);
#2133=EDGE_CURVE('',#1716,#1708,#1024,.T.);
#2134=EDGE_CURVE('',#1717,#1717,#1441,.T.);
#2135=EDGE_CURVE('',#1717,#1716,#1025,.T.);
#2136=EDGE_CURVE('',#1718,#1718,#1442,.T.);
#2137=EDGE_CURVE('',#1719,#1719,#1443,.F.);
#2138=EDGE_CURVE('',#1719,#1718,#1026,.T.);
#2139=EDGE_CURVE('',#1709,#1719,#1027,.T.);
#2140=EDGE_CURVE('',#1720,#1721,#1028,.T.);
#2141=EDGE_CURVE('',#1721,#1710,#1029,.T.);
#2142=EDGE_CURVE('',#1720,#1711,#1030,.T.);
#2143=EDGE_CURVE('',#1721,#1722,#1031,.T.);
#2144=EDGE_CURVE('',#1722,#1712,#1032,.T.);
#2145=EDGE_CURVE('',#1722,#1723,#1033,.T.);
#2146=EDGE_CURVE('',#1723,#1713,#1034,.T.);
#2147=EDGE_CURVE('',#1723,#1724,#1035,.T.);
#2148=EDGE_CURVE('',#1724,#1714,#1036,.T.);
#2149=EDGE_CURVE('',#1724,#1725,#1037,.T.);
#2150=EDGE_CURVE('',#1725,#1715,#1038,.T.);
#2151=EDGE_CURVE('',#1725,#1720,#1039,.T.);
#2152=ORIENTED_EDGE('',*,*,#1726,.F.);
#2153=ORIENTED_EDGE('',*,*,#1727,.T.);
#2154=ORIENTED_EDGE('',*,*,#1728,.F.);
#2155=ORIENTED_EDGE('',*,*,#1727,.F.);
#2156=ORIENTED_EDGE('',*,*,#1729,.F.);
#2157=ORIENTED_EDGE('',*,*,#1730,.T.);
#2158=ORIENTED_EDGE('',*,*,#1731,.F.);
#2159=ORIENTED_EDGE('',*,*,#1730,.F.);
#2160=ORIENTED_EDGE('',*,*,#1732,.F.);
#2161=ORIENTED_EDGE('',*,*,#1733,.T.);
#2162=ORIENTED_EDGE('',*,*,#1734,.F.);
#2163=ORIENTED_EDGE('',*,*,#1733,.F.);
#2164=ORIENTED_EDGE('',*,*,#1735,.T.);
#2165=ORIENTED_EDGE('',*,*,#1736,.T.);
#2166=ORIENTED_EDGE('',*,*,#1737,.F.);
#2167=ORIENTED_EDGE('',*,*,#1738,.F.);
#2168=ORIENTED_EDGE('',*,*,#1739,.T.);
#2169=ORIENTED_EDGE('',*,*,#1738,.T.);
#2170=ORIENTED_EDGE('',*,*,#1740,.F.);
#2171=ORIENTED_EDGE('',*,*,#1741,.F.);
#2172=ORIENTED_EDGE('',*,*,#1742,.T.);
#2173=ORIENTED_EDGE('',*,*,#1741,.T.);
#2174=ORIENTED_EDGE('',*,*,#1743,.F.);
#2175=ORIENTED_EDGE('',*,*,#1744,.F.);
#2176=ORIENTED_EDGE('',*,*,#1745,.T.);
#2177=ORIENTED_EDGE('',*,*,#1744,.T.);
#2178=ORIENTED_EDGE('',*,*,#1746,.F.);
#2179=ORIENTED_EDGE('',*,*,#1736,.F.);
#2180=ORIENTED_EDGE('',*,*,#1746,.T.);
#2181=ORIENTED_EDGE('',*,*,#1743,.T.);
#2182=ORIENTED_EDGE('',*,*,#1740,.T.);
#2183=ORIENTED_EDGE('',*,*,#1737,.T.);
#2184=ORIENTED_EDGE('',*,*,#1728,.T.);
#2185=ORIENTED_EDGE('',*,*,#1731,.T.);
#2186=ORIENTED_EDGE('',*,*,#1734,.T.);
#2187=ORIENTED_EDGE('',*,*,#1745,.F.);
#2188=ORIENTED_EDGE('',*,*,#1735,.F.);
#2189=ORIENTED_EDGE('',*,*,#1739,.F.);
#2190=ORIENTED_EDGE('',*,*,#1742,.F.);
#2191=ORIENTED_EDGE('',*,*,#1726,.T.);
#2192=ORIENTED_EDGE('',*,*,#1729,.T.);
#2193=ORIENTED_EDGE('',*,*,#1732,.T.);
#2194=ORIENTED_EDGE('',*,*,#1747,.F.);
#2195=ORIENTED_EDGE('',*,*,#1748,.F.);
#2196=ORIENTED_EDGE('',*,*,#1749,.F.);
#2197=ORIENTED_EDGE('',*,*,#1750,.F.);
#2198=ORIENTED_EDGE('',*,*,#1751,.T.);
#2199=ORIENTED_EDGE('',*,*,#1752,.F.);
#2200=ORIENTED_EDGE('',*,*,#1753,.F.);
#2201=ORIENTED_EDGE('',*,*,#1754,.F.);
#2202=ORIENTED_EDGE('',*,*,#1755,.T.);
#2203=ORIENTED_EDGE('',*,*,#1756,.F.);
#2204=ORIENTED_EDGE('',*,*,#1757,.F.);
#2205=ORIENTED_EDGE('',*,*,#1758,.F.);
#2206=ORIENTED_EDGE('',*,*,#1759,.F.);
#2207=ORIENTED_EDGE('',*,*,#1760,.F.);
#2208=ORIENTED_EDGE('',*,*,#1751,.F.);
#2209=ORIENTED_EDGE('',*,*,#1761,.F.);
#2210=ORIENTED_EDGE('',*,*,#1762,.F.);
#2211=ORIENTED_EDGE('',*,*,#1763,.F.);
#2212=ORIENTED_EDGE('',*,*,#1748,.T.);
#2213=ORIENTED_EDGE('',*,*,#1764,.F.);
#2214=ORIENTED_EDGE('',*,*,#1765,.F.);
#2215=ORIENTED_EDGE('',*,*,#1766,.F.);
#2216=ORIENTED_EDGE('',*,*,#1767,.F.);
#2217=ORIENTED_EDGE('',*,*,#1755,.F.);
#2218=ORIENTED_EDGE('',*,*,#1768,.F.);
#2219=ORIENTED_EDGE('',*,*,#1769,.F.);
#2220=ORIENTED_EDGE('',*,*,#1770,.F.);
#2221=ORIENTED_EDGE('',*,*,#1759,.T.);
#2222=ORIENTED_EDGE('',*,*,#1765,.T.);
#2223=ORIENTED_EDGE('',*,*,#1771,.T.);
#2224=ORIENTED_EDGE('',*,*,#1772,.F.);
#2225=ORIENTED_EDGE('',*,*,#1773,.F.);
#2226=ORIENTED_EDGE('',*,*,#1764,.T.);
#2227=ORIENTED_EDGE('',*,*,#1747,.T.);
#2228=ORIENTED_EDGE('',*,*,#1774,.F.);
#2229=ORIENTED_EDGE('',*,*,#1775,.T.);
#2230=ORIENTED_EDGE('',*,*,#1776,.F.);
#2231=ORIENTED_EDGE('',*,*,#1771,.F.);
#2232=ORIENTED_EDGE('',*,*,#1762,.T.);
#2233=ORIENTED_EDGE('',*,*,#1777,.T.);
#2234=ORIENTED_EDGE('',*,*,#1778,.F.);
#2235=ORIENTED_EDGE('',*,*,#1779,.F.);
#2236=ORIENTED_EDGE('',*,*,#1780,.F.);
#2237=ORIENTED_EDGE('',*,*,#1761,.T.);
#2238=ORIENTED_EDGE('',*,*,#1750,.T.);
#2239=ORIENTED_EDGE('',*,*,#1781,.F.);
#2240=ORIENTED_EDGE('',*,*,#1782,.T.);
#2241=ORIENTED_EDGE('',*,*,#1783,.F.);
#2242=ORIENTED_EDGE('',*,*,#1777,.F.);
#2243=ORIENTED_EDGE('',*,*,#1749,.T.);
#2244=ORIENTED_EDGE('',*,*,#1763,.T.);
#2245=ORIENTED_EDGE('',*,*,#1780,.T.);
#2246=ORIENTED_EDGE('',*,*,#1784,.T.);
#2247=ORIENTED_EDGE('',*,*,#1785,.T.);
#2248=ORIENTED_EDGE('',*,*,#1786,.T.);
#2249=ORIENTED_EDGE('',*,*,#1787,.F.);
#2250=ORIENTED_EDGE('',*,*,#1788,.F.);
#2251=ORIENTED_EDGE('',*,*,#1789,.T.);
#2252=ORIENTED_EDGE('',*,*,#1790,.T.);
#2253=ORIENTED_EDGE('',*,*,#1791,.T.);
#2254=ORIENTED_EDGE('',*,*,#1774,.T.);
#2255=ORIENTED_EDGE('',*,*,#1769,.T.);
#2256=ORIENTED_EDGE('',*,*,#1792,.T.);
#2257=ORIENTED_EDGE('',*,*,#1793,.T.);
#2258=ORIENTED_EDGE('',*,*,#1794,.T.);
#2259=ORIENTED_EDGE('',*,*,#1795,.T.);
#2260=ORIENTED_EDGE('',*,*,#1796,.T.);
#2261=ORIENTED_EDGE('',*,*,#1797,.F.);
#2262=ORIENTED_EDGE('',*,*,#1798,.F.);
#2263=ORIENTED_EDGE('',*,*,#1799,.T.);
#2264=ORIENTED_EDGE('',*,*,#1800,.T.);
#2265=ORIENTED_EDGE('',*,*,#1801,.T.);
#2266=ORIENTED_EDGE('',*,*,#1802,.T.);
#2267=ORIENTED_EDGE('',*,*,#1803,.T.);
#2268=ORIENTED_EDGE('',*,*,#1804,.T.);
#2269=ORIENTED_EDGE('',*,*,#1805,.T.);
#2270=ORIENTED_EDGE('',*,*,#1806,.T.);
#2271=ORIENTED_EDGE('',*,*,#1807,.T.);
#2272=ORIENTED_EDGE('',*,*,#1808,.F.);
#2273=ORIENTED_EDGE('',*,*,#1809,.F.);
#2274=ORIENTED_EDGE('',*,*,#1810,.T.);
#2275=ORIENTED_EDGE('',*,*,#1811,.T.);
#2276=ORIENTED_EDGE('',*,*,#1812,.T.);
#2277=ORIENTED_EDGE('',*,*,#1813,.T.);
#2278=ORIENTED_EDGE('',*,*,#1781,.T.);
#2279=ORIENTED_EDGE('',*,*,#1753,.T.);
#2280=ORIENTED_EDGE('',*,*,#1814,.T.);
#2281=ORIENTED_EDGE('',*,*,#1815,.T.);
#2282=ORIENTED_EDGE('',*,*,#1816,.F.);
#2283=ORIENTED_EDGE('',*,*,#1817,.T.);
#2284=ORIENTED_EDGE('',*,*,#1818,.F.);
#2285=ORIENTED_EDGE('',*,*,#1819,.F.);
#2286=ORIENTED_EDGE('',*,*,#1820,.F.);
#2287=ORIENTED_EDGE('',*,*,#1821,.T.);
#2288=ORIENTED_EDGE('',*,*,#1822,.F.);
#2289=ORIENTED_EDGE('',*,*,#1817,.F.);
#2290=ORIENTED_EDGE('',*,*,#1823,.F.);
#2291=ORIENTED_EDGE('',*,*,#1824,.T.);
#2292=ORIENTED_EDGE('',*,*,#1825,.F.);
#2293=ORIENTED_EDGE('',*,*,#1821,.F.);
#2294=ORIENTED_EDGE('',*,*,#1754,.T.);
#2295=ORIENTED_EDGE('',*,*,#1773,.T.);
#2296=ORIENTED_EDGE('',*,*,#1826,.F.);
#2297=ORIENTED_EDGE('',*,*,#1824,.F.);
#2298=ORIENTED_EDGE('',*,*,#1827,.F.);
#2299=ORIENTED_EDGE('',*,*,#1766,.T.);
#2300=ORIENTED_EDGE('',*,*,#1791,.F.);
#2301=ORIENTED_EDGE('',*,*,#1828,.T.);
#2302=ORIENTED_EDGE('',*,*,#1829,.F.);
#2303=ORIENTED_EDGE('',*,*,#1775,.F.);
#2304=ORIENTED_EDGE('',*,*,#1790,.F.);
#2305=ORIENTED_EDGE('',*,*,#1830,.T.);
#2306=ORIENTED_EDGE('',*,*,#1831,.F.);
#2307=ORIENTED_EDGE('',*,*,#1828,.F.);
#2308=ORIENTED_EDGE('',*,*,#1789,.F.);
#2309=ORIENTED_EDGE('',*,*,#1832,.F.);
#2310=ORIENTED_EDGE('',*,*,#1833,.F.);
#2311=ORIENTED_EDGE('',*,*,#1830,.F.);
#2312=ORIENTED_EDGE('',*,*,#1796,.F.);
#2313=ORIENTED_EDGE('',*,*,#1834,.T.);
#2314=ORIENTED_EDGE('',*,*,#1835,.F.);
#2315=ORIENTED_EDGE('',*,*,#1836,.F.);
#2316=ORIENTED_EDGE('',*,*,#1795,.F.);
#2317=ORIENTED_EDGE('',*,*,#1837,.T.);
#2318=ORIENTED_EDGE('',*,*,#1838,.F.);
#2319=ORIENTED_EDGE('',*,*,#1834,.F.);
#2320=ORIENTED_EDGE('',*,*,#1794,.F.);
#2321=ORIENTED_EDGE('',*,*,#1839,.T.);
#2322=ORIENTED_EDGE('',*,*,#1840,.F.);
#2323=ORIENTED_EDGE('',*,*,#1837,.F.);
#2324=ORIENTED_EDGE('',*,*,#1793,.F.);
#2325=ORIENTED_EDGE('',*,*,#1841,.T.);
#2326=ORIENTED_EDGE('',*,*,#1842,.F.);
#2327=ORIENTED_EDGE('',*,*,#1839,.F.);
#2328=ORIENTED_EDGE('',*,*,#1758,.T.);
#2329=ORIENTED_EDGE('',*,*,#1843,.T.);
#2330=ORIENTED_EDGE('',*,*,#1844,.F.);
#2331=ORIENTED_EDGE('',*,*,#1841,.F.);
#2332=ORIENTED_EDGE('',*,*,#1792,.F.);
#2333=ORIENTED_EDGE('',*,*,#1768,.T.);
#2334=ORIENTED_EDGE('',*,*,#1757,.T.);
#2335=ORIENTED_EDGE('',*,*,#1845,.F.);
#2336=ORIENTED_EDGE('',*,*,#1846,.T.);
#2337=ORIENTED_EDGE('',*,*,#1847,.F.);
#2338=ORIENTED_EDGE('',*,*,#1843,.F.);
#2339=ORIENTED_EDGE('',*,*,#1848,.F.);
#2340=ORIENTED_EDGE('',*,*,#1849,.T.);
#2341=ORIENTED_EDGE('',*,*,#1850,.F.);
#2342=ORIENTED_EDGE('',*,*,#1846,.F.);
#2343=ORIENTED_EDGE('',*,*,#1851,.F.);
#2344=ORIENTED_EDGE('',*,*,#1852,.T.);
#2345=ORIENTED_EDGE('',*,*,#1853,.F.);
#2346=ORIENTED_EDGE('',*,*,#1849,.F.);
#2347=ORIENTED_EDGE('',*,*,#1854,.F.);
#2348=ORIENTED_EDGE('',*,*,#1855,.F.);
#2349=ORIENTED_EDGE('',*,*,#1856,.F.);
#2350=ORIENTED_EDGE('',*,*,#1852,.F.);
#2351=ORIENTED_EDGE('',*,*,#1807,.F.);
#2352=ORIENTED_EDGE('',*,*,#1857,.T.);
#2353=ORIENTED_EDGE('',*,*,#1858,.F.);
#2354=ORIENTED_EDGE('',*,*,#1859,.F.);
#2355=ORIENTED_EDGE('',*,*,#1806,.F.);
#2356=ORIENTED_EDGE('',*,*,#1860,.T.);
#2357=ORIENTED_EDGE('',*,*,#1861,.F.);
#2358=ORIENTED_EDGE('',*,*,#1857,.F.);
#2359=ORIENTED_EDGE('',*,*,#1805,.F.);
#2360=ORIENTED_EDGE('',*,*,#1862,.T.);
#2361=ORIENTED_EDGE('',*,*,#1863,.F.);
#2362=ORIENTED_EDGE('',*,*,#1860,.F.);
#2363=ORIENTED_EDGE('',*,*,#1804,.F.);
#2364=ORIENTED_EDGE('',*,*,#1864,.T.);
#2365=ORIENTED_EDGE('',*,*,#1865,.F.);
#2366=ORIENTED_EDGE('',*,*,#1862,.F.);
#2367=ORIENTED_EDGE('',*,*,#1803,.F.);
#2368=ORIENTED_EDGE('',*,*,#1866,.T.);
#2369=ORIENTED_EDGE('',*,*,#1867,.F.);
#2370=ORIENTED_EDGE('',*,*,#1864,.F.);
#2371=ORIENTED_EDGE('',*,*,#1802,.F.);
#2372=ORIENTED_EDGE('',*,*,#1868,.T.);
#2373=ORIENTED_EDGE('',*,*,#1869,.F.);
#2374=ORIENTED_EDGE('',*,*,#1866,.F.);
#2375=ORIENTED_EDGE('',*,*,#1801,.F.);
#2376=ORIENTED_EDGE('',*,*,#1870,.T.);
#2377=ORIENTED_EDGE('',*,*,#1871,.F.);
#2378=ORIENTED_EDGE('',*,*,#1868,.F.);
#2379=ORIENTED_EDGE('',*,*,#1800,.F.);
#2380=ORIENTED_EDGE('',*,*,#1872,.T.);
#2381=ORIENTED_EDGE('',*,*,#1873,.F.);
#2382=ORIENTED_EDGE('',*,*,#1870,.F.);
#2383=ORIENTED_EDGE('',*,*,#1799,.F.);
#2384=ORIENTED_EDGE('',*,*,#1874,.F.);
#2385=ORIENTED_EDGE('',*,*,#1875,.F.);
#2386=ORIENTED_EDGE('',*,*,#1872,.F.);
#2387=ORIENTED_EDGE('',*,*,#1786,.F.);
#2388=ORIENTED_EDGE('',*,*,#1876,.T.);
#2389=ORIENTED_EDGE('',*,*,#1877,.F.);
#2390=ORIENTED_EDGE('',*,*,#1878,.F.);
#2391=ORIENTED_EDGE('',*,*,#1785,.F.);
#2392=ORIENTED_EDGE('',*,*,#1879,.T.);
#2393=ORIENTED_EDGE('',*,*,#1880,.F.);
#2394=ORIENTED_EDGE('',*,*,#1876,.F.);
#2395=ORIENTED_EDGE('',*,*,#1784,.F.);
#2396=ORIENTED_EDGE('',*,*,#1779,.T.);
#2397=ORIENTED_EDGE('',*,*,#1881,.F.);
#2398=ORIENTED_EDGE('',*,*,#1879,.F.);
#2399=ORIENTED_EDGE('',*,*,#1813,.F.);
#2400=ORIENTED_EDGE('',*,*,#1882,.T.);
#2401=ORIENTED_EDGE('',*,*,#1883,.F.);
#2402=ORIENTED_EDGE('',*,*,#1782,.F.);
#2403=ORIENTED_EDGE('',*,*,#1812,.F.);
#2404=ORIENTED_EDGE('',*,*,#1884,.T.);
#2405=ORIENTED_EDGE('',*,*,#1885,.F.);
#2406=ORIENTED_EDGE('',*,*,#1882,.F.);
#2407=ORIENTED_EDGE('',*,*,#1811,.F.);
#2408=ORIENTED_EDGE('',*,*,#1886,.T.);
#2409=ORIENTED_EDGE('',*,*,#1887,.F.);
#2410=ORIENTED_EDGE('',*,*,#1884,.F.);
#2411=ORIENTED_EDGE('',*,*,#1810,.F.);
#2412=ORIENTED_EDGE('',*,*,#1888,.F.);
#2413=ORIENTED_EDGE('',*,*,#1889,.F.);
#2414=ORIENTED_EDGE('',*,*,#1886,.F.);
#2415=ORIENTED_EDGE('',*,*,#1770,.T.);
#2416=ORIENTED_EDGE('',*,*,#1815,.F.);
#2417=ORIENTED_EDGE('',*,*,#1890,.T.);
#2418=ORIENTED_EDGE('',*,*,#1891,.F.);
#2419=ORIENTED_EDGE('',*,*,#1890,.F.);
#2420=ORIENTED_EDGE('',*,*,#1814,.F.);
#2421=ORIENTED_EDGE('',*,*,#1752,.T.);
#2422=ORIENTED_EDGE('',*,*,#1760,.T.);
#2423=ORIENTED_EDGE('',*,*,#1832,.T.);
#2424=ORIENTED_EDGE('',*,*,#1788,.T.);
#2425=ORIENTED_EDGE('',*,*,#1892,.T.);
#2426=ORIENTED_EDGE('',*,*,#1893,.F.);
#2427=ORIENTED_EDGE('',*,*,#1819,.T.);
#2428=ORIENTED_EDGE('',*,*,#1894,.F.);
#2429=ORIENTED_EDGE('',*,*,#1895,.F.);
#2430=ORIENTED_EDGE('',*,*,#1896,.T.);
#2431=ORIENTED_EDGE('',*,*,#1855,.T.);
#2432=ORIENTED_EDGE('',*,*,#1897,.T.);
#2433=ORIENTED_EDGE('',*,*,#1895,.T.);
#2434=ORIENTED_EDGE('',*,*,#1898,.F.);
#2435=ORIENTED_EDGE('',*,*,#1836,.T.);
#2436=ORIENTED_EDGE('',*,*,#1899,.F.);
#2437=ORIENTED_EDGE('',*,*,#1900,.F.);
#2438=ORIENTED_EDGE('',*,*,#1797,.T.);
#2439=ORIENTED_EDGE('',*,*,#1874,.T.);
#2440=ORIENTED_EDGE('',*,*,#1798,.T.);
#2441=ORIENTED_EDGE('',*,*,#1900,.T.);
#2442=ORIENTED_EDGE('',*,*,#1901,.F.);
#2443=ORIENTED_EDGE('',*,*,#1859,.T.);
#2444=ORIENTED_EDGE('',*,*,#1902,.F.);
#2445=ORIENTED_EDGE('',*,*,#1903,.F.);
#2446=ORIENTED_EDGE('',*,*,#1808,.T.);
#2447=ORIENTED_EDGE('',*,*,#1888,.T.);
#2448=ORIENTED_EDGE('',*,*,#1809,.T.);
#2449=ORIENTED_EDGE('',*,*,#1903,.T.);
#2450=ORIENTED_EDGE('',*,*,#1904,.F.);
#2451=ORIENTED_EDGE('',*,*,#1878,.T.);
#2452=ORIENTED_EDGE('',*,*,#1905,.F.);
#2453=ORIENTED_EDGE('',*,*,#1892,.F.);
#2454=ORIENTED_EDGE('',*,*,#1787,.T.);
#2455=ORIENTED_EDGE('',*,*,#1818,.T.);
#2456=ORIENTED_EDGE('',*,*,#1822,.T.);
#2457=ORIENTED_EDGE('',*,*,#1825,.T.);
#2458=ORIENTED_EDGE('',*,*,#1826,.T.);
#2459=ORIENTED_EDGE('',*,*,#1772,.T.);
#2460=ORIENTED_EDGE('',*,*,#1776,.T.);
#2461=ORIENTED_EDGE('',*,*,#1829,.T.);
#2462=ORIENTED_EDGE('',*,*,#1831,.T.);
#2463=ORIENTED_EDGE('',*,*,#1833,.T.);
#2464=ORIENTED_EDGE('',*,*,#1893,.T.);
#2465=ORIENTED_EDGE('',*,*,#1905,.T.);
#2466=ORIENTED_EDGE('',*,*,#1877,.T.);
#2467=ORIENTED_EDGE('',*,*,#1880,.T.);
#2468=ORIENTED_EDGE('',*,*,#1881,.T.);
#2469=ORIENTED_EDGE('',*,*,#1778,.T.);
#2470=ORIENTED_EDGE('',*,*,#1783,.T.);
#2471=ORIENTED_EDGE('',*,*,#1883,.T.);
#2472=ORIENTED_EDGE('',*,*,#1885,.T.);
#2473=ORIENTED_EDGE('',*,*,#1887,.T.);
#2474=ORIENTED_EDGE('',*,*,#1889,.T.);
#2475=ORIENTED_EDGE('',*,*,#1904,.T.);
#2476=ORIENTED_EDGE('',*,*,#1902,.T.);
#2477=ORIENTED_EDGE('',*,*,#1858,.T.);
#2478=ORIENTED_EDGE('',*,*,#1861,.T.);
#2479=ORIENTED_EDGE('',*,*,#1863,.T.);
#2480=ORIENTED_EDGE('',*,*,#1865,.T.);
#2481=ORIENTED_EDGE('',*,*,#1867,.T.);
#2482=ORIENTED_EDGE('',*,*,#1869,.T.);
#2483=ORIENTED_EDGE('',*,*,#1871,.T.);
#2484=ORIENTED_EDGE('',*,*,#1873,.T.);
#2485=ORIENTED_EDGE('',*,*,#1875,.T.);
#2486=ORIENTED_EDGE('',*,*,#1901,.T.);
#2487=ORIENTED_EDGE('',*,*,#1899,.T.);
#2488=ORIENTED_EDGE('',*,*,#1835,.T.);
#2489=ORIENTED_EDGE('',*,*,#1838,.T.);
#2490=ORIENTED_EDGE('',*,*,#1840,.T.);
#2491=ORIENTED_EDGE('',*,*,#1842,.T.);
#2492=ORIENTED_EDGE('',*,*,#1844,.T.);
#2493=ORIENTED_EDGE('',*,*,#1847,.T.);
#2494=ORIENTED_EDGE('',*,*,#1850,.T.);
#2495=ORIENTED_EDGE('',*,*,#1853,.T.);
#2496=ORIENTED_EDGE('',*,*,#1856,.T.);
#2497=ORIENTED_EDGE('',*,*,#1898,.T.);
#2498=ORIENTED_EDGE('',*,*,#1894,.T.);
#2499=ORIENTED_EDGE('',*,*,#1891,.T.);
#2500=ORIENTED_EDGE('',*,*,#1767,.T.);
#2501=ORIENTED_EDGE('',*,*,#1827,.T.);
#2502=ORIENTED_EDGE('',*,*,#1823,.T.);
#2503=ORIENTED_EDGE('',*,*,#1820,.T.);
#2504=ORIENTED_EDGE('',*,*,#1816,.T.);
#2505=ORIENTED_EDGE('',*,*,#1896,.F.);
#2506=ORIENTED_EDGE('',*,*,#1897,.F.);
#2507=ORIENTED_EDGE('',*,*,#1854,.T.);
#2508=ORIENTED_EDGE('',*,*,#1851,.T.);
#2509=ORIENTED_EDGE('',*,*,#1848,.T.);
#2510=ORIENTED_EDGE('',*,*,#1845,.T.);
#2511=ORIENTED_EDGE('',*,*,#1756,.T.);
#2512=ORIENTED_EDGE('',*,*,#1906,.F.);
#2513=ORIENTED_EDGE('',*,*,#1907,.T.);
#2514=ORIENTED_EDGE('',*,*,#1908,.F.);
#2515=ORIENTED_EDGE('',*,*,#1909,.F.);
#2516=ORIENTED_EDGE('',*,*,#1910,.T.);
#2517=ORIENTED_EDGE('',*,*,#1911,.F.);
#2518=ORIENTED_EDGE('',*,*,#1912,.F.);
#2519=ORIENTED_EDGE('',*,*,#1910,.F.);
#2520=ORIENTED_EDGE('',*,*,#1913,.F.);
#2521=ORIENTED_EDGE('',*,*,#1914,.T.);
#2522=ORIENTED_EDGE('',*,*,#1915,.F.);
#2523=ORIENTED_EDGE('',*,*,#1916,.T.);
#2524=ORIENTED_EDGE('',*,*,#1917,.F.);
#2525=ORIENTED_EDGE('',*,*,#1907,.F.);
#2526=ORIENTED_EDGE('',*,*,#1918,.F.);
#2527=ORIENTED_EDGE('',*,*,#1919,.F.);
#2528=ORIENTED_EDGE('',*,*,#1914,.F.);
#2529=ORIENTED_EDGE('',*,*,#1920,.F.);
#2530=ORIENTED_EDGE('',*,*,#1921,.F.);
#2531=ORIENTED_EDGE('',*,*,#1916,.F.);
#2532=ORIENTED_EDGE('',*,*,#1918,.T.);
#2533=ORIENTED_EDGE('',*,*,#1915,.T.);
#2534=ORIENTED_EDGE('',*,*,#1906,.T.);
#2535=ORIENTED_EDGE('',*,*,#1922,.F.);
#2536=ORIENTED_EDGE('',*,*,#1923,.T.);
#2537=ORIENTED_EDGE('',*,*,#1924,.T.);
#2538=ORIENTED_EDGE('',*,*,#1925,.F.);
#2539=ORIENTED_EDGE('',*,*,#1926,.T.);
#2540=ORIENTED_EDGE('',*,*,#1927,.F.);
#2541=ORIENTED_EDGE('',*,*,#1928,.T.);
#2542=ORIENTED_EDGE('',*,*,#1929,.T.);
#2543=ORIENTED_EDGE('',*,*,#1930,.F.);
#2544=ORIENTED_EDGE('',*,*,#1931,.T.);
#2545=ORIENTED_EDGE('',*,*,#1920,.T.);
#2546=ORIENTED_EDGE('',*,*,#1913,.T.);
#2547=ORIENTED_EDGE('',*,*,#1909,.T.);
#2548=ORIENTED_EDGE('',*,*,#1932,.F.);
#2549=ORIENTED_EDGE('',*,*,#1933,.T.);
#2550=ORIENTED_EDGE('',*,*,#1934,.T.);
#2551=ORIENTED_EDGE('',*,*,#1935,.F.);
#2552=ORIENTED_EDGE('',*,*,#1936,.F.);
#2553=ORIENTED_EDGE('',*,*,#1937,.F.);
#2554=ORIENTED_EDGE('',*,*,#1938,.F.);
#2555=ORIENTED_EDGE('',*,*,#1939,.T.);
#2556=ORIENTED_EDGE('',*,*,#1940,.F.);
#2557=ORIENTED_EDGE('',*,*,#1941,.F.);
#2558=ORIENTED_EDGE('',*,*,#1933,.F.);
#2559=ORIENTED_EDGE('',*,*,#1942,.F.);
#2560=ORIENTED_EDGE('',*,*,#1943,.F.);
#2561=ORIENTED_EDGE('',*,*,#1934,.F.);
#2562=ORIENTED_EDGE('',*,*,#1941,.T.);
#2563=ORIENTED_EDGE('',*,*,#1939,.F.);
#2564=ORIENTED_EDGE('',*,*,#1944,.T.);
#2565=ORIENTED_EDGE('',*,*,#1945,.F.);
#2566=ORIENTED_EDGE('',*,*,#1944,.F.);
#2567=ORIENTED_EDGE('',*,*,#1946,.F.);
#2568=ORIENTED_EDGE('',*,*,#1947,.T.);
#2569=ORIENTED_EDGE('',*,*,#1931,.F.);
#2570=ORIENTED_EDGE('',*,*,#1947,.F.);
#2571=ORIENTED_EDGE('',*,*,#1928,.F.);
#2572=ORIENTED_EDGE('',*,*,#1948,.F.);
#2573=ORIENTED_EDGE('',*,*,#1949,.F.);
#2574=ORIENTED_EDGE('',*,*,#1950,.F.);
#2575=ORIENTED_EDGE('',*,*,#1929,.F.);
#2576=ORIENTED_EDGE('',*,*,#1950,.T.);
#2577=ORIENTED_EDGE('',*,*,#1951,.F.);
#2578=ORIENTED_EDGE('',*,*,#1919,.T.);
#2579=ORIENTED_EDGE('',*,*,#1930,.T.);
#2580=ORIENTED_EDGE('',*,*,#1951,.T.);
#2581=ORIENTED_EDGE('',*,*,#1949,.T.);
#2582=ORIENTED_EDGE('',*,*,#1952,.F.);
#2583=ORIENTED_EDGE('',*,*,#1953,.F.);
#2584=ORIENTED_EDGE('',*,*,#1954,.F.);
#2585=ORIENTED_EDGE('',*,*,#1955,.T.);
#2586=ORIENTED_EDGE('',*,*,#1956,.T.);
#2587=ORIENTED_EDGE('',*,*,#1922,.T.);
#2588=ORIENTED_EDGE('',*,*,#1911,.T.);
#2589=ORIENTED_EDGE('',*,*,#1912,.T.);
#2590=ORIENTED_EDGE('',*,*,#1945,.T.);
#2591=ORIENTED_EDGE('',*,*,#1955,.F.);
#2592=ORIENTED_EDGE('',*,*,#1957,.F.);
#2593=ORIENTED_EDGE('',*,*,#1924,.F.);
#2594=ORIENTED_EDGE('',*,*,#1958,.T.);
#2595=ORIENTED_EDGE('',*,*,#1956,.F.);
#2596=ORIENTED_EDGE('',*,*,#1958,.F.);
#2597=ORIENTED_EDGE('',*,*,#1923,.F.);
#2598=ORIENTED_EDGE('',*,*,#1943,.T.);
#2599=ORIENTED_EDGE('',*,*,#1959,.T.);
#2600=ORIENTED_EDGE('',*,*,#1960,.T.);
#2601=ORIENTED_EDGE('',*,*,#1925,.T.);
#2602=ORIENTED_EDGE('',*,*,#1957,.T.);
#2603=ORIENTED_EDGE('',*,*,#1954,.T.);
#2604=ORIENTED_EDGE('',*,*,#1961,.T.);
#2605=ORIENTED_EDGE('',*,*,#1935,.T.);
#2606=ORIENTED_EDGE('',*,*,#1921,.T.);
#2607=ORIENTED_EDGE('',*,*,#1938,.T.);
#2608=ORIENTED_EDGE('',*,*,#1962,.F.);
#2609=ORIENTED_EDGE('',*,*,#1963,.F.);
#2610=ORIENTED_EDGE('',*,*,#1959,.F.);
#2611=ORIENTED_EDGE('',*,*,#1942,.T.);
#2612=ORIENTED_EDGE('',*,*,#1940,.T.);
#2613=ORIENTED_EDGE('',*,*,#1932,.T.);
#2614=ORIENTED_EDGE('',*,*,#1908,.T.);
#2615=ORIENTED_EDGE('',*,*,#1917,.T.);
#2616=ORIENTED_EDGE('',*,*,#1946,.T.);
#2617=ORIENTED_EDGE('',*,*,#1963,.T.);
#2618=ORIENTED_EDGE('',*,*,#1964,.F.);
#2619=ORIENTED_EDGE('',*,*,#1926,.F.);
#2620=ORIENTED_EDGE('',*,*,#1960,.F.);
#2621=ORIENTED_EDGE('',*,*,#1953,.T.);
#2622=ORIENTED_EDGE('',*,*,#1965,.F.);
#2623=ORIENTED_EDGE('',*,*,#1936,.T.);
#2624=ORIENTED_EDGE('',*,*,#1961,.F.);
#2625=ORIENTED_EDGE('',*,*,#1927,.T.);
#2626=ORIENTED_EDGE('',*,*,#1964,.T.);
#2627=ORIENTED_EDGE('',*,*,#1962,.T.);
#2628=ORIENTED_EDGE('',*,*,#1937,.T.);
#2629=ORIENTED_EDGE('',*,*,#1965,.T.);
#2630=ORIENTED_EDGE('',*,*,#1952,.T.);
#2631=ORIENTED_EDGE('',*,*,#1948,.T.);
#2632=ORIENTED_EDGE('',*,*,#1966,.F.);
#2633=ORIENTED_EDGE('',*,*,#1967,.F.);
#2634=ORIENTED_EDGE('',*,*,#1968,.F.);
#2635=ORIENTED_EDGE('',*,*,#1969,.F.);
#2636=ORIENTED_EDGE('',*,*,#1970,.F.);
#2637=ORIENTED_EDGE('',*,*,#1971,.F.);
#2638=ORIENTED_EDGE('',*,*,#1972,.F.);
#2639=ORIENTED_EDGE('',*,*,#1973,.F.);
#2640=ORIENTED_EDGE('',*,*,#1974,.F.);
#2641=ORIENTED_EDGE('',*,*,#1975,.T.);
#2642=ORIENTED_EDGE('',*,*,#1966,.T.);
#2643=ORIENTED_EDGE('',*,*,#1975,.F.);
#2644=ORIENTED_EDGE('',*,*,#1976,.F.);
#2645=ORIENTED_EDGE('',*,*,#1977,.T.);
#2646=ORIENTED_EDGE('',*,*,#1974,.T.);
#2647=ORIENTED_EDGE('',*,*,#1977,.F.);
#2648=ORIENTED_EDGE('',*,*,#1976,.T.);
#2649=ORIENTED_EDGE('',*,*,#1978,.F.);
#2650=ORIENTED_EDGE('',*,*,#1979,.F.);
#2651=ORIENTED_EDGE('',*,*,#1980,.T.);
#2652=ORIENTED_EDGE('',*,*,#1978,.T.);
#2653=ORIENTED_EDGE('',*,*,#1980,.F.);
#2654=ORIENTED_EDGE('',*,*,#1967,.T.);
#2655=ORIENTED_EDGE('',*,*,#1981,.T.);
#2656=ORIENTED_EDGE('',*,*,#1979,.T.);
#2657=ORIENTED_EDGE('',*,*,#1981,.F.);
#2658=ORIENTED_EDGE('',*,*,#1982,.T.);
#2659=ORIENTED_EDGE('',*,*,#1983,.T.);
#2660=ORIENTED_EDGE('',*,*,#1968,.T.);
#2661=ORIENTED_EDGE('',*,*,#1984,.F.);
#2662=ORIENTED_EDGE('',*,*,#1985,.T.);
#2663=ORIENTED_EDGE('',*,*,#1986,.T.);
#2664=ORIENTED_EDGE('',*,*,#1969,.T.);
#2665=ORIENTED_EDGE('',*,*,#1983,.F.);
#2666=ORIENTED_EDGE('',*,*,#1987,.T.);
#2667=ORIENTED_EDGE('',*,*,#1988,.T.);
#2668=ORIENTED_EDGE('',*,*,#1970,.T.);
#2669=ORIENTED_EDGE('',*,*,#1986,.F.);
#2670=ORIENTED_EDGE('',*,*,#1989,.T.);
#2671=ORIENTED_EDGE('',*,*,#1990,.T.);
#2672=ORIENTED_EDGE('',*,*,#1971,.T.);
#2673=ORIENTED_EDGE('',*,*,#1988,.F.);
#2674=ORIENTED_EDGE('',*,*,#1991,.T.);
#2675=ORIENTED_EDGE('',*,*,#1992,.T.);
#2676=ORIENTED_EDGE('',*,*,#1972,.T.);
#2677=ORIENTED_EDGE('',*,*,#1990,.F.);
#2678=ORIENTED_EDGE('',*,*,#1993,.T.);
#2679=ORIENTED_EDGE('',*,*,#1984,.T.);
#2680=ORIENTED_EDGE('',*,*,#1973,.T.);
#2681=ORIENTED_EDGE('',*,*,#1992,.F.);
#2682=ORIENTED_EDGE('',*,*,#1993,.F.);
#2683=ORIENTED_EDGE('',*,*,#1991,.F.);
#2684=ORIENTED_EDGE('',*,*,#1989,.F.);
#2685=ORIENTED_EDGE('',*,*,#1987,.F.);
#2686=ORIENTED_EDGE('',*,*,#1985,.F.);
#2687=ORIENTED_EDGE('',*,*,#1982,.F.);
#2688=ORIENTED_EDGE('',*,*,#1994,.T.);
#2689=ORIENTED_EDGE('',*,*,#1995,.T.);
#2690=ORIENTED_EDGE('',*,*,#1996,.T.);
#2691=ORIENTED_EDGE('',*,*,#1995,.F.);
#2692=ORIENTED_EDGE('',*,*,#1994,.F.);
#2693=ORIENTED_EDGE('',*,*,#1997,.F.);
#2694=ORIENTED_EDGE('',*,*,#1998,.T.);
#2695=ORIENTED_EDGE('',*,*,#1996,.F.);
#2696=ORIENTED_EDGE('',*,*,#1998,.F.);
#2697=ORIENTED_EDGE('',*,*,#1999,.F.);
#2698=ORIENTED_EDGE('',*,*,#2000,.F.);
#2699=ORIENTED_EDGE('',*,*,#2001,.F.);
#2700=ORIENTED_EDGE('',*,*,#2002,.F.);
#2701=ORIENTED_EDGE('',*,*,#2001,.T.);
#2702=ORIENTED_EDGE('',*,*,#2003,.T.);
#2703=ORIENTED_EDGE('',*,*,#2004,.F.);
#2704=ORIENTED_EDGE('',*,*,#2005,.T.);
#2705=ORIENTED_EDGE('',*,*,#2000,.T.);
#2706=ORIENTED_EDGE('',*,*,#2006,.T.);
#2707=ORIENTED_EDGE('',*,*,#2007,.F.);
#2708=ORIENTED_EDGE('',*,*,#2003,.F.);
#2709=ORIENTED_EDGE('',*,*,#1999,.T.);
#2710=ORIENTED_EDGE('',*,*,#2008,.F.);
#2711=ORIENTED_EDGE('',*,*,#2009,.F.);
#2712=ORIENTED_EDGE('',*,*,#2006,.F.);
#2713=ORIENTED_EDGE('',*,*,#2002,.T.);
#2714=ORIENTED_EDGE('',*,*,#2005,.F.);
#2715=ORIENTED_EDGE('',*,*,#2010,.F.);
#2716=ORIENTED_EDGE('',*,*,#2008,.T.);
#2717=ORIENTED_EDGE('',*,*,#1997,.T.);
#2718=ORIENTED_EDGE('',*,*,#2007,.T.);
#2719=ORIENTED_EDGE('',*,*,#2009,.T.);
#2720=ORIENTED_EDGE('',*,*,#2010,.T.);
#2721=ORIENTED_EDGE('',*,*,#2004,.T.);
#2722=ORIENTED_EDGE('',*,*,#2011,.F.);
#2723=ORIENTED_EDGE('',*,*,#2012,.F.);
#2724=ORIENTED_EDGE('',*,*,#2013,.F.);
#2725=ORIENTED_EDGE('',*,*,#2012,.T.);
#2726=ORIENTED_EDGE('',*,*,#2014,.F.);
#2727=ORIENTED_EDGE('',*,*,#2015,.F.);
#2728=ORIENTED_EDGE('',*,*,#2015,.T.);
#2729=ORIENTED_EDGE('',*,*,#2011,.T.);
#2730=ORIENTED_EDGE('',*,*,#2013,.T.);
#2731=ORIENTED_EDGE('',*,*,#2016,.F.);
#2732=ORIENTED_EDGE('',*,*,#2017,.F.);
#2733=ORIENTED_EDGE('',*,*,#2018,.T.);
#2734=ORIENTED_EDGE('',*,*,#2016,.T.);
#2735=ORIENTED_EDGE('',*,*,#2018,.F.);
#2736=ORIENTED_EDGE('',*,*,#2019,.F.);
#2737=ORIENTED_EDGE('',*,*,#2020,.T.);
#2738=ORIENTED_EDGE('',*,*,#2017,.T.);
#2739=ORIENTED_EDGE('',*,*,#2020,.F.);
#2740=ORIENTED_EDGE('',*,*,#2019,.T.);
#2741=ORIENTED_EDGE('',*,*,#2014,.T.);
#2742=ORIENTED_EDGE('',*,*,#2021,.T.);
#2743=ORIENTED_EDGE('',*,*,#2022,.T.);
#2744=ORIENTED_EDGE('',*,*,#2023,.T.);
#2745=ORIENTED_EDGE('',*,*,#2024,.T.);
#2746=ORIENTED_EDGE('',*,*,#2025,.T.);
#2747=ORIENTED_EDGE('',*,*,#2026,.T.);
#2748=ORIENTED_EDGE('',*,*,#2027,.F.);
#2749=ORIENTED_EDGE('',*,*,#2028,.T.);
#2750=ORIENTED_EDGE('',*,*,#2029,.T.);
#2751=ORIENTED_EDGE('',*,*,#2026,.F.);
#2752=ORIENTED_EDGE('',*,*,#2030,.F.);
#2753=ORIENTED_EDGE('',*,*,#2031,.T.);
#2754=ORIENTED_EDGE('',*,*,#2030,.T.);
#2755=ORIENTED_EDGE('',*,*,#2025,.F.);
#2756=ORIENTED_EDGE('',*,*,#2032,.F.);
#2757=ORIENTED_EDGE('',*,*,#2033,.T.);
#2758=ORIENTED_EDGE('',*,*,#2032,.T.);
#2759=ORIENTED_EDGE('',*,*,#2024,.F.);
#2760=ORIENTED_EDGE('',*,*,#2034,.F.);
#2761=ORIENTED_EDGE('',*,*,#2035,.T.);
#2762=ORIENTED_EDGE('',*,*,#2034,.T.);
#2763=ORIENTED_EDGE('',*,*,#2023,.F.);
#2764=ORIENTED_EDGE('',*,*,#2036,.F.);
#2765=ORIENTED_EDGE('',*,*,#2037,.T.);
#2766=ORIENTED_EDGE('',*,*,#2036,.T.);
#2767=ORIENTED_EDGE('',*,*,#2022,.F.);
#2768=ORIENTED_EDGE('',*,*,#2038,.F.);
#2769=ORIENTED_EDGE('',*,*,#2039,.T.);
#2770=ORIENTED_EDGE('',*,*,#2038,.T.);
#2771=ORIENTED_EDGE('',*,*,#2021,.F.);
#2772=ORIENTED_EDGE('',*,*,#2029,.F.);
#2773=ORIENTED_EDGE('',*,*,#2040,.F.);
#2774=ORIENTED_EDGE('',*,*,#2041,.T.);
#2775=ORIENTED_EDGE('',*,*,#2042,.F.);
#2776=ORIENTED_EDGE('',*,*,#2041,.F.);
#2777=ORIENTED_EDGE('',*,*,#2039,.F.);
#2778=ORIENTED_EDGE('',*,*,#2028,.F.);
#2779=ORIENTED_EDGE('',*,*,#2031,.F.);
#2780=ORIENTED_EDGE('',*,*,#2033,.F.);
#2781=ORIENTED_EDGE('',*,*,#2035,.F.);
#2782=ORIENTED_EDGE('',*,*,#2037,.F.);
#2783=ORIENTED_EDGE('',*,*,#2040,.T.);
#2784=ORIENTED_EDGE('',*,*,#2043,.F.);
#2785=ORIENTED_EDGE('',*,*,#2044,.T.);
#2786=ORIENTED_EDGE('',*,*,#2027,.T.);
#2787=ORIENTED_EDGE('',*,*,#2044,.F.);
#2788=ORIENTED_EDGE('',*,*,#2045,.F.);
#2789=ORIENTED_EDGE('',*,*,#2046,.T.);
#2790=ORIENTED_EDGE('',*,*,#2043,.T.);
#2791=ORIENTED_EDGE('',*,*,#2046,.F.);
#2792=ORIENTED_EDGE('',*,*,#2045,.T.);
#2793=ORIENTED_EDGE('',*,*,#2042,.T.);
#2794=ORIENTED_EDGE('',*,*,#2047,.T.);
#2795=ORIENTED_EDGE('',*,*,#2047,.F.);
#2796=ORIENTED_EDGE('',*,*,#2048,.F.);
#2797=ORIENTED_EDGE('',*,*,#2049,.T.);
#2798=ORIENTED_EDGE('',*,*,#2050,.T.);
#2799=ORIENTED_EDGE('',*,*,#2049,.F.);
#2800=ORIENTED_EDGE('',*,*,#2050,.F.);
#2801=ORIENTED_EDGE('',*,*,#2048,.T.);
#2802=ORIENTED_EDGE('',*,*,#2051,.F.);
#2803=ORIENTED_EDGE('',*,*,#2052,.T.);
#2804=ORIENTED_EDGE('',*,*,#2053,.T.);
#2805=ORIENTED_EDGE('',*,*,#2052,.F.);
#2806=ORIENTED_EDGE('',*,*,#2053,.F.);
#2807=ORIENTED_EDGE('',*,*,#2054,.F.);
#2808=ORIENTED_EDGE('',*,*,#2051,.T.);
#2809=ORIENTED_EDGE('',*,*,#2055,.F.);
#2810=ORIENTED_EDGE('',*,*,#2055,.T.);
#2811=ORIENTED_EDGE('',*,*,#2056,.T.);
#2812=ORIENTED_EDGE('',*,*,#2057,.T.);
#2813=ORIENTED_EDGE('',*,*,#2056,.F.);
#2814=ORIENTED_EDGE('',*,*,#2058,.F.);
#2815=ORIENTED_EDGE('',*,*,#2059,.F.);
#2816=ORIENTED_EDGE('',*,*,#2060,.T.);
#2817=ORIENTED_EDGE('',*,*,#2061,.F.);
#2818=ORIENTED_EDGE('',*,*,#2060,.F.);
#2819=ORIENTED_EDGE('',*,*,#2062,.F.);
#2820=ORIENTED_EDGE('',*,*,#2063,.F.);
#2821=ORIENTED_EDGE('',*,*,#2064,.F.);
#2822=ORIENTED_EDGE('',*,*,#2065,.F.);
#2823=ORIENTED_EDGE('',*,*,#2066,.F.);
#2824=ORIENTED_EDGE('',*,*,#2067,.T.);
#2825=ORIENTED_EDGE('',*,*,#2068,.F.);
#2826=ORIENTED_EDGE('',*,*,#2069,.F.);
#2827=ORIENTED_EDGE('',*,*,#2070,.F.);
#2828=ORIENTED_EDGE('',*,*,#2071,.F.);
#2829=ORIENTED_EDGE('',*,*,#2072,.F.);
#2830=ORIENTED_EDGE('',*,*,#2073,.F.);
#2831=ORIENTED_EDGE('',*,*,#2067,.F.);
#2832=ORIENTED_EDGE('',*,*,#2063,.T.);
#2833=ORIENTED_EDGE('',*,*,#2074,.T.);
#2834=ORIENTED_EDGE('',*,*,#2072,.T.);
#2835=ORIENTED_EDGE('',*,*,#2075,.F.);
#2836=ORIENTED_EDGE('',*,*,#2062,.T.);
#2837=ORIENTED_EDGE('',*,*,#2076,.T.);
#2838=ORIENTED_EDGE('',*,*,#2073,.T.);
#2839=ORIENTED_EDGE('',*,*,#2074,.F.);
#2840=ORIENTED_EDGE('',*,*,#2059,.T.);
#2841=ORIENTED_EDGE('',*,*,#2077,.T.);
#2842=ORIENTED_EDGE('',*,*,#2068,.T.);
#2843=ORIENTED_EDGE('',*,*,#2076,.F.);
#2844=ORIENTED_EDGE('',*,*,#2078,.F.);
#2845=ORIENTED_EDGE('',*,*,#2079,.T.);
#2846=ORIENTED_EDGE('',*,*,#2054,.T.);
#2847=ORIENTED_EDGE('',*,*,#2079,.F.);
#2848=ORIENTED_EDGE('',*,*,#2058,.T.);
#2849=ORIENTED_EDGE('',*,*,#2080,.T.);
#2850=ORIENTED_EDGE('',*,*,#2069,.T.);
#2851=ORIENTED_EDGE('',*,*,#2077,.F.);
#2852=ORIENTED_EDGE('',*,*,#2064,.T.);
#2853=ORIENTED_EDGE('',*,*,#2075,.T.);
#2854=ORIENTED_EDGE('',*,*,#2071,.T.);
#2855=ORIENTED_EDGE('',*,*,#2081,.F.);
#2856=ORIENTED_EDGE('',*,*,#2065,.T.);
#2857=ORIENTED_EDGE('',*,*,#2081,.T.);
#2858=ORIENTED_EDGE('',*,*,#2070,.T.);
#2859=ORIENTED_EDGE('',*,*,#2080,.F.);
#2860=ORIENTED_EDGE('',*,*,#2066,.T.);
#2861=ORIENTED_EDGE('',*,*,#2078,.T.);
#2862=ORIENTED_EDGE('',*,*,#2061,.T.);
#2863=ORIENTED_EDGE('',*,*,#2057,.F.);
#2864=ORIENTED_EDGE('',*,*,#2082,.F.);
#2865=ORIENTED_EDGE('',*,*,#2083,.F.);
#2866=ORIENTED_EDGE('',*,*,#2084,.F.);
#2867=ORIENTED_EDGE('',*,*,#2085,.F.);
#2868=ORIENTED_EDGE('',*,*,#2086,.F.);
#2869=ORIENTED_EDGE('',*,*,#2087,.F.);
#2870=ORIENTED_EDGE('',*,*,#2088,.F.);
#2871=ORIENTED_EDGE('',*,*,#2089,.F.);
#2872=ORIENTED_EDGE('',*,*,#2090,.F.);
#2873=ORIENTED_EDGE('',*,*,#2091,.F.);
#2874=ORIENTED_EDGE('',*,*,#2092,.F.);
#2875=ORIENTED_EDGE('',*,*,#2083,.T.);
#2876=ORIENTED_EDGE('',*,*,#2093,.F.);
#2877=ORIENTED_EDGE('',*,*,#2094,.F.);
#2878=ORIENTED_EDGE('',*,*,#2095,.F.);
#2879=ORIENTED_EDGE('',*,*,#2087,.T.);
#2880=ORIENTED_EDGE('',*,*,#2085,.T.);
#2881=ORIENTED_EDGE('',*,*,#2096,.F.);
#2882=ORIENTED_EDGE('',*,*,#2097,.F.);
#2883=ORIENTED_EDGE('',*,*,#2098,.F.);
#2884=ORIENTED_EDGE('',*,*,#2089,.T.);
#2885=ORIENTED_EDGE('',*,*,#2099,.F.);
#2886=ORIENTED_EDGE('',*,*,#2100,.T.);
#2887=ORIENTED_EDGE('',*,*,#2101,.F.);
#2888=ORIENTED_EDGE('',*,*,#2082,.T.);
#2889=ORIENTED_EDGE('',*,*,#2098,.T.);
#2890=ORIENTED_EDGE('',*,*,#2102,.T.);
#2891=ORIENTED_EDGE('',*,*,#2103,.T.);
#2892=ORIENTED_EDGE('',*,*,#2104,.T.);
#2893=ORIENTED_EDGE('',*,*,#2090,.T.);
#2894=ORIENTED_EDGE('',*,*,#2088,.T.);
#2895=ORIENTED_EDGE('',*,*,#2095,.T.);
#2896=ORIENTED_EDGE('',*,*,#2105,.T.);
#2897=ORIENTED_EDGE('',*,*,#2106,.T.);
#2898=ORIENTED_EDGE('',*,*,#2107,.T.);
#2899=ORIENTED_EDGE('',*,*,#2099,.T.);
#2900=ORIENTED_EDGE('',*,*,#2108,.T.);
#2901=ORIENTED_EDGE('',*,*,#2109,.T.);
#2902=ORIENTED_EDGE('',*,*,#2110,.T.);
#2903=ORIENTED_EDGE('',*,*,#2111,.T.);
#2904=ORIENTED_EDGE('',*,*,#2112,.T.);
#2905=ORIENTED_EDGE('',*,*,#2113,.T.);
#2906=ORIENTED_EDGE('',*,*,#2094,.T.);
#2907=ORIENTED_EDGE('',*,*,#2114,.F.);
#2908=ORIENTED_EDGE('',*,*,#2091,.T.);
#2909=ORIENTED_EDGE('',*,*,#2104,.F.);
#2910=ORIENTED_EDGE('',*,*,#2115,.F.);
#2911=ORIENTED_EDGE('',*,*,#2112,.F.);
#2912=ORIENTED_EDGE('',*,*,#2116,.F.);
#2913=ORIENTED_EDGE('',*,*,#2105,.F.);
#2914=ORIENTED_EDGE('',*,*,#2111,.F.);
#2915=ORIENTED_EDGE('',*,*,#2117,.F.);
#2916=ORIENTED_EDGE('',*,*,#2106,.F.);
#2917=ORIENTED_EDGE('',*,*,#2116,.T.);
#2918=ORIENTED_EDGE('',*,*,#2113,.F.);
#2919=ORIENTED_EDGE('',*,*,#2115,.T.);
#2920=ORIENTED_EDGE('',*,*,#2103,.F.);
#2921=ORIENTED_EDGE('',*,*,#2118,.F.);
#2922=ORIENTED_EDGE('',*,*,#2108,.F.);
#2923=ORIENTED_EDGE('',*,*,#2118,.T.);
#2924=ORIENTED_EDGE('',*,*,#2102,.F.);
#2925=ORIENTED_EDGE('',*,*,#2097,.T.);
#2926=ORIENTED_EDGE('',*,*,#2119,.F.);
#2927=ORIENTED_EDGE('',*,*,#2120,.F.);
#2928=ORIENTED_EDGE('',*,*,#2109,.F.);
#2929=ORIENTED_EDGE('',*,*,#2120,.T.);
#2930=ORIENTED_EDGE('',*,*,#2121,.F.);
#2931=ORIENTED_EDGE('',*,*,#2122,.F.);
#2932=ORIENTED_EDGE('',*,*,#2110,.F.);
#2933=ORIENTED_EDGE('',*,*,#2122,.T.);
#2934=ORIENTED_EDGE('',*,*,#2123,.F.);
#2935=ORIENTED_EDGE('',*,*,#2100,.F.);
#2936=ORIENTED_EDGE('',*,*,#2107,.F.);
#2937=ORIENTED_EDGE('',*,*,#2117,.T.);
#2938=ORIENTED_EDGE('',*,*,#2086,.T.);
#2939=ORIENTED_EDGE('',*,*,#2101,.T.);
#2940=ORIENTED_EDGE('',*,*,#2123,.T.);
#2941=ORIENTED_EDGE('',*,*,#2121,.T.);
#2942=ORIENTED_EDGE('',*,*,#2119,.T.);
#2943=ORIENTED_EDGE('',*,*,#2096,.T.);
#2944=ORIENTED_EDGE('',*,*,#2084,.T.);
#2945=ORIENTED_EDGE('',*,*,#2092,.T.);
#2946=ORIENTED_EDGE('',*,*,#2114,.T.);
#2947=ORIENTED_EDGE('',*,*,#2093,.T.);
#2948=ORIENTED_EDGE('',*,*,#2124,.F.);
#2949=ORIENTED_EDGE('',*,*,#2125,.F.);
#2950=ORIENTED_EDGE('',*,*,#2126,.F.);
#2951=ORIENTED_EDGE('',*,*,#2127,.F.);
#2952=ORIENTED_EDGE('',*,*,#2128,.F.);
#2953=ORIENTED_EDGE('',*,*,#2129,.F.);
#2954=ORIENTED_EDGE('',*,*,#2130,.F.);
#2955=ORIENTED_EDGE('',*,*,#2131,.F.);
#2956=ORIENTED_EDGE('',*,*,#2132,.F.);
#2957=ORIENTED_EDGE('',*,*,#2133,.T.);
#2958=ORIENTED_EDGE('',*,*,#2124,.T.);
#2959=ORIENTED_EDGE('',*,*,#2133,.F.);
#2960=ORIENTED_EDGE('',*,*,#2134,.F.);
#2961=ORIENTED_EDGE('',*,*,#2135,.T.);
#2962=ORIENTED_EDGE('',*,*,#2132,.T.);
#2963=ORIENTED_EDGE('',*,*,#2135,.F.);
#2964=ORIENTED_EDGE('',*,*,#2134,.T.);
#2965=ORIENTED_EDGE('',*,*,#2136,.F.);
#2966=ORIENTED_EDGE('',*,*,#2137,.F.);
#2967=ORIENTED_EDGE('',*,*,#2138,.T.);
#2968=ORIENTED_EDGE('',*,*,#2136,.T.);
#2969=ORIENTED_EDGE('',*,*,#2138,.F.);
#2970=ORIENTED_EDGE('',*,*,#2125,.T.);
#2971=ORIENTED_EDGE('',*,*,#2139,.T.);
#2972=ORIENTED_EDGE('',*,*,#2137,.T.);
#2973=ORIENTED_EDGE('',*,*,#2139,.F.);
#2974=ORIENTED_EDGE('',*,*,#2140,.T.);
#2975=ORIENTED_EDGE('',*,*,#2141,.T.);
#2976=ORIENTED_EDGE('',*,*,#2126,.T.);
#2977=ORIENTED_EDGE('',*,*,#2142,.F.);
#2978=ORIENTED_EDGE('',*,*,#2143,.T.);
#2979=ORIENTED_EDGE('',*,*,#2144,.T.);
#2980=ORIENTED_EDGE('',*,*,#2127,.T.);
#2981=ORIENTED_EDGE('',*,*,#2141,.F.);
#2982=ORIENTED_EDGE('',*,*,#2145,.T.);
#2983=ORIENTED_EDGE('',*,*,#2146,.T.);
#2984=ORIENTED_EDGE('',*,*,#2128,.T.);
#2985=ORIENTED_EDGE('',*,*,#2144,.F.);
#2986=ORIENTED_EDGE('',*,*,#2147,.T.);
#2987=ORIENTED_EDGE('',*,*,#2148,.T.);
#2988=ORIENTED_EDGE('',*,*,#2129,.T.);
#2989=ORIENTED_EDGE('',*,*,#2146,.F.);
#2990=ORIENTED_EDGE('',*,*,#2149,.T.);
#2991=ORIENTED_EDGE('',*,*,#2150,.T.);
#2992=ORIENTED_EDGE('',*,*,#2130,.T.);
#2993=ORIENTED_EDGE('',*,*,#2148,.F.);
#2994=ORIENTED_EDGE('',*,*,#2151,.T.);
#2995=ORIENTED_EDGE('',*,*,#2142,.T.);
#2996=ORIENTED_EDGE('',*,*,#2131,.T.);
#2997=ORIENTED_EDGE('',*,*,#2150,.F.);
#2998=ORIENTED_EDGE('',*,*,#2151,.F.);
#2999=ORIENTED_EDGE('',*,*,#2149,.F.);
#3000=ORIENTED_EDGE('',*,*,#2147,.F.);
#3001=ORIENTED_EDGE('',*,*,#2145,.F.);
#3002=ORIENTED_EDGE('',*,*,#2143,.F.);
#3003=ORIENTED_EDGE('',*,*,#2140,.F.);
#3004=CYLINDRICAL_SURFACE('',#3329,0.275);
#3005=CYLINDRICAL_SURFACE('',#3332,0.275);
#3006=CYLINDRICAL_SURFACE('',#3335,0.34);
#3007=CYLINDRICAL_SURFACE('',#3349,0.5);
#3008=CYLINDRICAL_SURFACE('',#3399,0.21);
#3009=CYLINDRICAL_SURFACE('',#3415,0.5);
#3010=CYLINDRICAL_SURFACE('',#3417,0.5);
#3011=CYLINDRICAL_SURFACE('',#3426,0.3);
#3012=CYLINDRICAL_SURFACE('',#3428,0.275);
#3013=CYLINDRICAL_SURFACE('',#3430,0.275);
#3014=CYLINDRICAL_SURFACE('',#3447,0.425);
#3015=CYLINDRICAL_SURFACE('',#3455,0.24505);
#3016=CYLINDRICAL_SURFACE('',#3469,2.);
#3017=CYLINDRICAL_SURFACE('',#3475,0.5);
#3018=CYLINDRICAL_SURFACE('',#3479,0.5);
#3019=CYLINDRICAL_SURFACE('',#3491,2.);
#3020=CYLINDRICAL_SURFACE('',#3505,0.3);
#3021=CYLINDRICAL_SURFACE('',#3509,0.3933);
#3022=CYLINDRICAL_SURFACE('',#3516,0.34);
#3023=CYLINDRICAL_SURFACE('',#3525,0.5);
#3024=CYLINDRICAL_SURFACE('',#3532,0.338975);
#3025=CYLINDRICAL_SURFACE('',#3541,0.338975);
#3026=CYLINDRICAL_SURFACE('',#3549,0.5);
#3027=CYLINDRICAL_SURFACE('',#3553,0.5);
#3028=CYLINDRICAL_SURFACE('',#3567,0.2117);
#3029=CYLINDRICAL_SURFACE('',#3582,0.425);
#3030=CYLINDRICAL_SURFACE('',#3590,0.24505);
#3031=ADVANCED_FACE('',(#337),#3004,.F.);
#3032=ADVANCED_FACE('',(#338),#3005,.F.);
#3033=ADVANCED_FACE('',(#339),#3006,.F.);
#3034=ADVANCED_FACE('',(#340),#201,.T.);
#3035=ADVANCED_FACE('',(#341),#202,.T.);
#3036=ADVANCED_FACE('',(#342),#203,.T.);
#3037=ADVANCED_FACE('',(#343),#204,.T.);
#3038=ADVANCED_FACE('',(#344,#177,#178,#179),#205,.T.);
#3039=ADVANCED_FACE('',(#345,#180,#181,#182),#206,.F.);
#3040=ADVANCED_FACE('',(#346),#207,.F.);
#3041=ADVANCED_FACE('',(#347),#208,.T.);
#3042=ADVANCED_FACE('',(#348),#3007,.F.);
#3043=ADVANCED_FACE('',(#349),#209,.F.);
#3044=ADVANCED_FACE('',(#350),#210,.T.);
#3045=ADVANCED_FACE('',(#351),#211,.F.);
#3046=ADVANCED_FACE('',(#352),#212,.F.);
#3047=ADVANCED_FACE('',(#353),#213,.F.);
#3048=ADVANCED_FACE('',(#354),#214,.F.);
#3049=ADVANCED_FACE('',(#355),#215,.F.);
#3050=ADVANCED_FACE('',(#356),#216,.F.);
#3051=ADVANCED_FACE('',(#357),#217,.F.);
#3052=ADVANCED_FACE('',(#358),#218,.F.);
#3053=ADVANCED_FACE('',(#359),#219,.F.);
#3054=ADVANCED_FACE('',(#360),#220,.F.);
#3055=ADVANCED_FACE('',(#361),#221,.F.);
#3056=ADVANCED_FACE('',(#362),#222,.F.);
#3057=ADVANCED_FACE('',(#363),#223,.F.);
#3058=ADVANCED_FACE('',(#364),#224,.F.);
#3059=ADVANCED_FACE('',(#365),#225,.F.);
#3060=ADVANCED_FACE('',(#366),#226,.F.);
#3061=ADVANCED_FACE('',(#367),#227,.F.);
#3062=ADVANCED_FACE('',(#368),#228,.F.);
#3063=ADVANCED_FACE('',(#369),#229,.F.);
#3064=ADVANCED_FACE('',(#370),#230,.F.);
#3065=ADVANCED_FACE('',(#371),#231,.F.);
#3066=ADVANCED_FACE('',(#372),#232,.F.);
#3067=ADVANCED_FACE('',(#373),#233,.F.);
#3068=ADVANCED_FACE('',(#374),#234,.F.);
#3069=ADVANCED_FACE('',(#375),#235,.F.);
#3070=ADVANCED_FACE('',(#376),#236,.F.);
#3071=ADVANCED_FACE('',(#377),#237,.F.);
#3072=ADVANCED_FACE('',(#378),#238,.F.);
#3073=ADVANCED_FACE('',(#379),#239,.F.);
#3074=ADVANCED_FACE('',(#380),#240,.F.);
#3075=ADVANCED_FACE('',(#381),#241,.F.);
#3076=ADVANCED_FACE('',(#382),#242,.F.);
#3077=ADVANCED_FACE('',(#383),#243,.F.);
#3078=ADVANCED_FACE('',(#384),#244,.F.);
#3079=ADVANCED_FACE('',(#385),#245,.F.);
#3080=ADVANCED_FACE('',(#386),#246,.F.);
#3081=ADVANCED_FACE('',(#387),#247,.F.);
#3082=ADVANCED_FACE('',(#388),#248,.F.);
#3083=ADVANCED_FACE('',(#389),#3008,.F.);
#3084=ADVANCED_FACE('',(#390),#249,.T.);
#3085=ADVANCED_FACE('',(#391),#250,.T.);
#3086=ADVANCED_FACE('',(#392),#251,.T.);
#3087=ADVANCED_FACE('',(#393),#252,.T.);
#3088=ADVANCED_FACE('',(#394),#253,.T.);
#3089=ADVANCED_FACE('',(#395),#254,.T.);
#3090=ADVANCED_FACE('',(#396),#255,.T.);
#3091=ADVANCED_FACE('',(#397),#256,.T.);
#3092=ADVANCED_FACE('',(#398,#183),#257,.T.);
#3093=ADVANCED_FACE('',(#399),#258,.F.);
#3094=ADVANCED_FACE('',(#400),#259,.T.);
#3095=ADVANCED_FACE('',(#401),#3009,.F.);
#3096=ADVANCED_FACE('',(#402),#3010,.F.);
#3097=ADVANCED_FACE('',(#403),#260,.F.);
#3098=ADVANCED_FACE('',(#404,#184),#261,.T.);
#3099=ADVANCED_FACE('',(#405,#185),#262,.T.);
#3100=ADVANCED_FACE('',(#406),#263,.F.);
#3101=ADVANCED_FACE('',(#407),#3011,.F.);
#3102=ADVANCED_FACE('',(#408),#3012,.F.);
#3103=ADVANCED_FACE('',(#409),#3013,.F.);
#3104=ADVANCED_FACE('',(#410),#264,.T.);
#3105=ADVANCED_FACE('',(#411),#265,.F.);
#3106=ADVANCED_FACE('',(#412,#186),#266,.T.);
#3107=ADVANCED_FACE('',(#413),#267,.T.);
#3108=ADVANCED_FACE('',(#414),#268,.T.);
#3109=ADVANCED_FACE('',(#415),#269,.T.);
#3110=ADVANCED_FACE('',(#416,#187),#270,.T.);
#3111=ADVANCED_FACE('',(#417),#271,.T.);
#3112=ADVANCED_FACE('',(#418),#272,.T.);
#3113=ADVANCED_FACE('',(#419),#273,.T.);
#3114=ADVANCED_FACE('',(#420),#274,.T.);
#3115=ADVANCED_FACE('',(#421,#188),#275,.F.);
#3116=ADVANCED_FACE('',(#422),#3014,.T.);
#3117=ADVANCED_FACE('',(#423),#119,.T.);
#3118=ADVANCED_FACE('',(#424,#189),#276,.T.);
#3119=ADVANCED_FACE('',(#425),#120,.T.);
#3120=ADVANCED_FACE('',(#426),#3015,.T.);
#3121=ADVANCED_FACE('',(#427),#277,.F.);
#3122=ADVANCED_FACE('',(#428),#278,.F.);
#3123=ADVANCED_FACE('',(#429),#279,.F.);
#3124=ADVANCED_FACE('',(#430),#280,.F.);
#3125=ADVANCED_FACE('',(#431),#281,.F.);
#3126=ADVANCED_FACE('',(#432),#282,.F.);
#3127=ADVANCED_FACE('',(#433),#283,.F.);
#3128=ADVANCED_FACE('',(#434),#121,.T.);
#3129=ADVANCED_FACE('',(#435),#284,.T.);
#3130=ADVANCED_FACE('',(#436),#3016,.T.);
#3131=ADVANCED_FACE('',(#437),#285,.F.);
#3132=ADVANCED_FACE('',(#438),#286,.T.);
#3133=ADVANCED_FACE('',(#439),#3017,.F.);
#3134=ADVANCED_FACE('',(#440),#287,.F.);
#3135=ADVANCED_FACE('',(#441),#3018,.F.);
#3136=ADVANCED_FACE('',(#442,#190),#288,.T.);
#3137=ADVANCED_FACE('',(#443),#289,.T.);
#3138=ADVANCED_FACE('',(#444),#290,.T.);
#3139=ADVANCED_FACE('',(#445,#191),#117,.F.);
#3140=ADVANCED_FACE('',(#446),#291,.T.);
#3141=ADVANCED_FACE('',(#447),#3019,.T.);
#3142=ADVANCED_FACE('',(#448),#122,.T.);
#3143=ADVANCED_FACE('',(#449,#192),#292,.T.);
#3144=ADVANCED_FACE('',(#450,#193),#293,.T.);
#3145=ADVANCED_FACE('',(#451),#294,.T.);
#3146=ADVANCED_FACE('',(#452),#295,.T.);
#3147=ADVANCED_FACE('',(#453),#296,.T.);
#3148=ADVANCED_FACE('',(#454),#297,.T.);
#3149=ADVANCED_FACE('',(#455),#298,.T.);
#3150=ADVANCED_FACE('',(#456),#299,.T.);
#3151=ADVANCED_FACE('',(#457),#3020,.T.);
#3152=ADVANCED_FACE('',(#458,#194),#300,.T.);
#3153=ADVANCED_FACE('',(#459),#3021,.T.);
#3154=ADVANCED_FACE('',(#460),#123,.T.);
#3155=ADVANCED_FACE('',(#461),#301,.T.);
#3156=ADVANCED_FACE('',(#462),#118,.T.);
#3157=ADVANCED_FACE('',(#463),#3022,.F.);
#3158=ADVANCED_FACE('',(#464),#302,.F.);
#3159=ADVANCED_FACE('',(#465),#303,.T.);
#3160=ADVANCED_FACE('',(#466),#3023,.F.);
#3161=ADVANCED_FACE('',(#467,#195),#304,.F.);
#3162=ADVANCED_FACE('',(#468,#196),#305,.T.);
#3163=ADVANCED_FACE('',(#469),#3024,.F.);
#3164=ADVANCED_FACE('',(#470),#124,.T.);
#3165=ADVANCED_FACE('',(#471),#125,.T.);
#3166=ADVANCED_FACE('',(#472),#306,.T.);
#3167=ADVANCED_FACE('',(#473),#307,.T.);
#3168=ADVANCED_FACE('',(#474),#308,.T.);
#3169=ADVANCED_FACE('',(#475),#3025,.F.);
#3170=ADVANCED_FACE('',(#476),#309,.T.);
#3171=ADVANCED_FACE('',(#477),#310,.T.);
#3172=ADVANCED_FACE('',(#478),#311,.T.);
#3173=ADVANCED_FACE('',(#479,#197),#312,.T.);
#3174=ADVANCED_FACE('',(#480,#198),#313,.F.);
#3175=ADVANCED_FACE('',(#481),#3026,.F.);
#3176=ADVANCED_FACE('',(#482),#3027,.F.);
#3177=ADVANCED_FACE('',(#483),#314,.T.);
#3178=ADVANCED_FACE('',(#484),#315,.T.);
#3179=ADVANCED_FACE('',(#485),#316,.T.);
#3180=ADVANCED_FACE('',(#486),#317,.T.);
#3181=ADVANCED_FACE('',(#487),#318,.T.);
#3182=ADVANCED_FACE('',(#488),#319,.T.);
#3183=ADVANCED_FACE('',(#489),#320,.T.);
#3184=ADVANCED_FACE('',(#490),#3028,.F.);
#3185=ADVANCED_FACE('',(#491),#321,.F.);
#3186=ADVANCED_FACE('',(#492),#322,.F.);
#3187=ADVANCED_FACE('',(#493),#323,.T.);
#3188=ADVANCED_FACE('',(#494),#324,.T.);
#3189=ADVANCED_FACE('',(#495),#325,.T.);
#3190=ADVANCED_FACE('',(#496),#326,.T.);
#3191=ADVANCED_FACE('',(#497),#327,.T.);
#3192=ADVANCED_FACE('',(#498,#199),#328,.F.);
#3193=ADVANCED_FACE('',(#499),#3029,.T.);
#3194=ADVANCED_FACE('',(#500),#126,.T.);
#3195=ADVANCED_FACE('',(#501,#200),#329,.T.);
#3196=ADVANCED_FACE('',(#502),#127,.T.);
#3197=ADVANCED_FACE('',(#503),#3030,.T.);
#3198=ADVANCED_FACE('',(#504),#330,.F.);
#3199=ADVANCED_FACE('',(#505),#331,.F.);
#3200=ADVANCED_FACE('',(#506),#332,.F.);
#3201=ADVANCED_FACE('',(#507),#333,.F.);
#3202=ADVANCED_FACE('',(#508),#334,.F.);
#3203=ADVANCED_FACE('',(#509),#335,.F.);
#3204=ADVANCED_FACE('',(#510),#336,.F.);
#3205=CLOSED_SHELL('',(#3031,#3032,#3033,#3034,#3035,#3036,#3037,#3038,
#3039));
#3206=CLOSED_SHELL('',(#3040,#3041,#3042,#3043,#3044,#3045,#3046,#3047,
#3048,#3049,#3050,#3051,#3052,#3053,#3054,#3055,#3056,#3057,#3058,#3059,
#3060,#3061,#3062,#3063,#3064,#3065,#3066,#3067,#3068,#3069,#3070,#3071,
#3072,#3073,#3074,#3075,#3076,#3077,#3078,#3079,#3080,#3081,#3082,#3083,
#3084,#3085,#3086,#3087,#3088,#3089,#3090,#3091,#3092,#3093));
#3207=CLOSED_SHELL('',(#3094,#3095,#3096,#3097,#3098,#3099,#3100,#3101,
#3102,#3103,#3104,#3105,#3106,#3107,#3108,#3109,#3110,#3111,#3112,#3113));
#3208=CLOSED_SHELL('',(#3114,#3115,#3116,#3117,#3118,#3119,#3120,#3121,
#3122,#3123,#3124,#3125,#3126,#3127));
#3209=CLOSED_SHELL('',(#3128,#3129,#3130,#3131,#3132,#3133,#3134,#3135,
#3136));
#3210=CLOSED_SHELL('',(#3137,#3138,#3139,#3140,#3141,#3142,#3143));
#3211=CLOSED_SHELL('',(#3144,#3145,#3146,#3147,#3148,#3149,#3150,#3151,
#3152,#3153,#3154,#3155,#3156));
#3212=CLOSED_SHELL('',(#3157,#3158,#3159));
#3213=CLOSED_SHELL('',(#3160,#3161,#3162,#3163,#3164,#3165,#3166,#3167,
#3168,#3169,#3170,#3171,#3172,#3173,#3174));
#3214=CLOSED_SHELL('',(#3175,#3176,#3177,#3178,#3179,#3180,#3181,#3182,
#3183,#3184,#3185,#3186,#3187,#3188,#3189,#3190));
#3215=CLOSED_SHELL('',(#3191,#3192,#3193,#3194,#3195,#3196,#3197,#3198,
#3199,#3200,#3201,#3202,#3203,#3204));
#3216=DERIVED_UNIT_ELEMENT(#3236,1.);
#3217=DERIVED_UNIT_ELEMENT(#5504,-3.);
#3218=DERIVED_UNIT_ELEMENT(#3236,1.);
#3219=DERIVED_UNIT_ELEMENT(#5504,-3.);
#3220=DERIVED_UNIT_ELEMENT(#3236,1.);
#3221=DERIVED_UNIT_ELEMENT(#5504,-3.);
#3222=DERIVED_UNIT_ELEMENT(#3236,1.);
#3223=DERIVED_UNIT_ELEMENT(#5504,-3.);
#3224=DERIVED_UNIT_ELEMENT(#3236,1.);
#3225=DERIVED_UNIT_ELEMENT(#5504,-3.);
#3226=DERIVED_UNIT_ELEMENT(#3236,1.);
#3227=DERIVED_UNIT_ELEMENT(#5504,-3.);
#3228=DERIVED_UNIT_ELEMENT(#3236,1.);
#3229=DERIVED_UNIT_ELEMENT(#5504,-3.);
#3230=DERIVED_UNIT_ELEMENT(#3236,1.);
#3231=DERIVED_UNIT_ELEMENT(#5504,-3.);
#3232=DERIVED_UNIT_ELEMENT(#3236,1.);
#3233=DERIVED_UNIT_ELEMENT(#5504,-3.);
#3234=DERIVED_UNIT_ELEMENT(#3236,1.);
#3235=DERIVED_UNIT_ELEMENT(#5504,-3.);
#3236=(
MASS_UNIT()
NAMED_UNIT(*)
SI_UNIT(.KILO.,.GRAM.)
);
#3237=DERIVED_UNIT((#3216,#3217));
#3238=DERIVED_UNIT((#3218,#3219));
#3239=DERIVED_UNIT((#3220,#3221));
#3240=DERIVED_UNIT((#3222,#3223));
#3241=DERIVED_UNIT((#3224,#3225));
#3242=DERIVED_UNIT((#3226,#3227));
#3243=DERIVED_UNIT((#3228,#3229));
#3244=DERIVED_UNIT((#3230,#3231));
#3245=DERIVED_UNIT((#3232,#3233));
#3246=DERIVED_UNIT((#3234,#3235));
#3247=MEASURE_REPRESENTATION_ITEM('density measure',
POSITIVE_RATIO_MEASURE(7850.),#3237);
#3248=MEASURE_REPRESENTATION_ITEM('density measure',
POSITIVE_RATIO_MEASURE(7850.),#3238);
#3249=MEASURE_REPRESENTATION_ITEM('density measure',
POSITIVE_RATIO_MEASURE(7850.),#3239);
#3250=MEASURE_REPRESENTATION_ITEM('density measure',
POSITIVE_RATIO_MEASURE(7850.),#3240);
#3251=MEASURE_REPRESENTATION_ITEM('density measure',
POSITIVE_RATIO_MEASURE(7850.),#3241);
#3252=MEASURE_REPRESENTATION_ITEM('density measure',
POSITIVE_RATIO_MEASURE(7850.),#3242);
#3253=MEASURE_REPRESENTATION_ITEM('density measure',
POSITIVE_RATIO_MEASURE(7850.),#3243);
#3254=MEASURE_REPRESENTATION_ITEM('density measure',
POSITIVE_RATIO_MEASURE(7850.),#3244);
#3255=MEASURE_REPRESENTATION_ITEM('density measure',
POSITIVE_RATIO_MEASURE(7850.),#3245);
#3256=MEASURE_REPRESENTATION_ITEM('density measure',
POSITIVE_RATIO_MEASURE(7850.),#3246);
#3257=PROPERTY_DEFINITION_REPRESENTATION(#3307,#3277);
#3258=PROPERTY_DEFINITION_REPRESENTATION(#3308,#3278);
#3259=PROPERTY_DEFINITION_REPRESENTATION(#3309,#3279);
#3260=PROPERTY_DEFINITION_REPRESENTATION(#3310,#3280);
#3261=PROPERTY_DEFINITION_REPRESENTATION(#3311,#3281);
#3262=PROPERTY_DEFINITION_REPRESENTATION(#3312,#3282);
#3263=PROPERTY_DEFINITION_REPRESENTATION(#3313,#3283);
#3264=PROPERTY_DEFINITION_REPRESENTATION(#3314,#3284);
#3265=PROPERTY_DEFINITION_REPRESENTATION(#3315,#3285);
#3266=PROPERTY_DEFINITION_REPRESENTATION(#3316,#3286);
#3267=PROPERTY_DEFINITION_REPRESENTATION(#3317,#3287);
#3268=PROPERTY_DEFINITION_REPRESENTATION(#3318,#3288);
#3269=PROPERTY_DEFINITION_REPRESENTATION(#3319,#3289);
#3270=PROPERTY_DEFINITION_REPRESENTATION(#3320,#3290);
#3271=PROPERTY_DEFINITION_REPRESENTATION(#3321,#3291);
#3272=PROPERTY_DEFINITION_REPRESENTATION(#3322,#3292);
#3273=PROPERTY_DEFINITION_REPRESENTATION(#3323,#3293);
#3274=PROPERTY_DEFINITION_REPRESENTATION(#3324,#3294);
#3275=PROPERTY_DEFINITION_REPRESENTATION(#3325,#3295);
#3276=PROPERTY_DEFINITION_REPRESENTATION(#3326,#3296);
#3277=REPRESENTATION('material name',(#3297),#5491);
#3278=REPRESENTATION('density',(#3247),#5491);
#3279=REPRESENTATION('material name',(#3298),#5492);
#3280=REPRESENTATION('density',(#3248),#5492);
#3281=REPRESENTATION('material name',(#3299),#5493);
#3282=REPRESENTATION('density',(#3249),#5493);
#3283=REPRESENTATION('material name',(#3300),#5494);
#3284=REPRESENTATION('density',(#3250),#5494);
#3285=REPRESENTATION('material name',(#3301),#5496);
#3286=REPRESENTATION('density',(#3251),#5496);
#3287=REPRESENTATION('material name',(#3302),#5497);
#3288=REPRESENTATION('density',(#3252),#5497);
#3289=REPRESENTATION('material name',(#3303),#5498);
#3290=REPRESENTATION('density',(#3253),#5498);
#3291=REPRESENTATION('material name',(#3304),#5499);
#3292=REPRESENTATION('density',(#3254),#5499);
#3293=REPRESENTATION('material name',(#3305),#5500);
#3294=REPRESENTATION('density',(#3255),#5500);
#3295=REPRESENTATION('material name',(#3306),#5501);
#3296=REPRESENTATION('density',(#3256),#5501);
#3297=DESCRIPTIVE_REPRESENTATION_ITEM('Steel','Steel');
#3298=DESCRIPTIVE_REPRESENTATION_ITEM('Steel','Steel');
#3299=DESCRIPTIVE_REPRESENTATION_ITEM('Steel','Steel');
#3300=DESCRIPTIVE_REPRESENTATION_ITEM('Steel','Steel');
#3301=DESCRIPTIVE_REPRESENTATION_ITEM('Steel','Steel');
#3302=DESCRIPTIVE_REPRESENTATION_ITEM('Steel','Steel');
#3303=DESCRIPTIVE_REPRESENTATION_ITEM('Steel','Steel');
#3304=DESCRIPTIVE_REPRESENTATION_ITEM('Steel','Steel');
#3305=DESCRIPTIVE_REPRESENTATION_ITEM('Steel','Steel');
#3306=DESCRIPTIVE_REPRESENTATION_ITEM('Steel','Steel');
#3307=PROPERTY_DEFINITION('material property','material name',#5568);
#3308=PROPERTY_DEFINITION('material property','density of part',#5568);
#3309=PROPERTY_DEFINITION('material property','material name',#5569);
#3310=PROPERTY_DEFINITION('material property','density of part',#5569);
#3311=PROPERTY_DEFINITION('material property','material name',#5570);
#3312=PROPERTY_DEFINITION('material property','density of part',#5570);
#3313=PROPERTY_DEFINITION('material property','material name',#5571);
#3314=PROPERTY_DEFINITION('material property','density of part',#5571);
#3315=PROPERTY_DEFINITION('material property','material name',#5573);
#3316=PROPERTY_DEFINITION('material property','density of part',#5573);
#3317=PROPERTY_DEFINITION('material property','material name',#5574);
#3318=PROPERTY_DEFINITION('material property','density of part',#5574);
#3319=PROPERTY_DEFINITION('material property','material name',#5575);
#3320=PROPERTY_DEFINITION('material property','density of part',#5575);
#3321=PROPERTY_DEFINITION('material property','material name',#5576);
#3322=PROPERTY_DEFINITION('material property','density of part',#5576);
#3323=PROPERTY_DEFINITION('material property','material name',#5577);
#3324=PROPERTY_DEFINITION('material property','density of part',#5577);
#3325=PROPERTY_DEFINITION('material property','material name',#5578);
#3326=PROPERTY_DEFINITION('material property','density of part',#5578);
#3327=AXIS2_PLACEMENT_3D('',#4531,#3618,#3619);
#3328=AXIS2_PLACEMENT_3D('',#4532,#3620,#3621);
#3329=AXIS2_PLACEMENT_3D('',#4533,#3622,#3623);
#3330=AXIS2_PLACEMENT_3D('',#4535,#3624,#3625);
#3331=AXIS2_PLACEMENT_3D('',#4538,#3627,#3628);
#3332=AXIS2_PLACEMENT_3D('',#4539,#3629,#3630);
#3333=AXIS2_PLACEMENT_3D('',#4541,#3631,#3632);
#3334=AXIS2_PLACEMENT_3D('',#4544,#3634,#3635);
#3335=AXIS2_PLACEMENT_3D('',#4545,#3636,#3637);
#3336=AXIS2_PLACEMENT_3D('',#4547,#3638,#3639);
#3337=AXIS2_PLACEMENT_3D('',#4550,#3641,#3642);
#3338=AXIS2_PLACEMENT_3D('',#4551,#3643,#3644);
#3339=AXIS2_PLACEMENT_3D('',#4560,#3649,#3650);
#3340=AXIS2_PLACEMENT_3D('',#4566,#3654,#3655);
#3341=AXIS2_PLACEMENT_3D('',#4572,#3659,#3660);
#3342=AXIS2_PLACEMENT_3D('',#4575,#3663,#3664);
#3343=AXIS2_PLACEMENT_3D('',#4576,#3665,#3666);
#3344=AXIS2_PLACEMENT_3D('',#4577,#3667,#3668);
#3345=AXIS2_PLACEMENT_3D('',#4578,#3669,#3670);
#3346=AXIS2_PLACEMENT_3D('',#4583,#3672,#3673);
#3347=AXIS2_PLACEMENT_3D('',#4585,#3675,#3676);
#3348=AXIS2_PLACEMENT_3D('',#4590,#3678,#3679);
#3349=AXIS2_PLACEMENT_3D('',#4594,#3682,#3683);
#3350=AXIS2_PLACEMENT_3D('',#4597,#3684,#3685);
#3351=AXIS2_PLACEMENT_3D('',#4599,#3686,#3687);
#3352=AXIS2_PLACEMENT_3D('',#4603,#3689,#3690);
#3353=AXIS2_PLACEMENT_3D('',#4607,#3692,#3693);
#3354=AXIS2_PLACEMENT_3D('',#4617,#3695,#3696);
#3355=AXIS2_PLACEMENT_3D('',#4620,#3698,#3699);
#3356=AXIS2_PLACEMENT_3D('',#4621,#3700,#3701);
#3357=AXIS2_PLACEMENT_3D('',#4622,#3702,#3703);
#3358=AXIS2_PLACEMENT_3D('',#4626,#3706,#3707);
#3359=AXIS2_PLACEMENT_3D('',#4632,#3711,#3712);
#3360=AXIS2_PLACEMENT_3D('',#4638,#3716,#3717);
#3361=AXIS2_PLACEMENT_3D('',#4644,#3721,#3722);
#3362=AXIS2_PLACEMENT_3D('',#4652,#3727,#3728);
#3363=AXIS2_PLACEMENT_3D('',#4658,#3732,#3733);
#3364=AXIS2_PLACEMENT_3D('',#4674,#3742,#3743);
#3365=AXIS2_PLACEMENT_3D('',#4719,#3766,#3767);
#3366=AXIS2_PLACEMENT_3D('',#4720,#3768,#3769);
#3367=AXIS2_PLACEMENT_3D('',#4721,#3770,#3771);
#3368=AXIS2_PLACEMENT_3D('',#4730,#3776,#3777);
#3369=AXIS2_PLACEMENT_3D('',#4736,#3781,#3782);
#3370=AXIS2_PLACEMENT_3D('',#4742,#3786,#3787);
#3371=AXIS2_PLACEMENT_3D('',#4745,#3790,#3791);
#3372=AXIS2_PLACEMENT_3D('',#4749,#3794,#3795);
#3373=AXIS2_PLACEMENT_3D('',#4753,#3798,#3799);
#3374=AXIS2_PLACEMENT_3D('',#4757,#3802,#3803);
#3375=AXIS2_PLACEMENT_3D('',#4763,#3807,#3808);
#3376=AXIS2_PLACEMENT_3D('',#4767,#3811,#3812);
#3377=AXIS2_PLACEMENT_3D('',#4771,#3815,#3816);
#3378=AXIS2_PLACEMENT_3D('',#4775,#3819,#3820);
#3379=AXIS2_PLACEMENT_3D('',#4779,#3823,#3824);
#3380=AXIS2_PLACEMENT_3D('',#4785,#3828,#3829);
#3381=AXIS2_PLACEMENT_3D('',#4791,#3833,#3834);
#3382=AXIS2_PLACEMENT_3D('',#4797,#3838,#3839);
#3383=AXIS2_PLACEMENT_3D('',#4803,#3843,#3844);
#3384=AXIS2_PLACEMENT_3D('',#4809,#3848,#3849);
#3385=AXIS2_PLACEMENT_3D('',#4813,#3852,#3853);
#3386=AXIS2_PLACEMENT_3D('',#4817,#3856,#3857);
#3387=AXIS2_PLACEMENT_3D('',#4821,#3860,#3861);
#3388=AXIS2_PLACEMENT_3D('',#4825,#3864,#3865);
#3389=AXIS2_PLACEMENT_3D('',#4829,#3868,#3869);
#3390=AXIS2_PLACEMENT_3D('',#4833,#3872,#3873);
#3391=AXIS2_PLACEMENT_3D('',#4837,#3876,#3877);
#3392=AXIS2_PLACEMENT_3D('',#4841,#3880,#3881);
#3393=AXIS2_PLACEMENT_3D('',#4847,#3885,#3886);
#3394=AXIS2_PLACEMENT_3D('',#4851,#3889,#3890);
#3395=AXIS2_PLACEMENT_3D('',#4853,#3892,#3893);
#3396=AXIS2_PLACEMENT_3D('',#4857,#3896,#3897);
#3397=AXIS2_PLACEMENT_3D('',#4861,#3900,#3901);
#3398=AXIS2_PLACEMENT_3D('',#4865,#3904,#3905);
#3399=AXIS2_PLACEMENT_3D('',#4869,#3908,#3909);
#3400=AXIS2_PLACEMENT_3D('',#4872,#3911,#3912);
#3401=AXIS2_PLACEMENT_3D('',#4873,#3913,#3914);
#3402=AXIS2_PLACEMENT_3D('',#4877,#3917,#3918);
#3403=AXIS2_PLACEMENT_3D('',#4883,#3922,#3923);
#3404=AXIS2_PLACEMENT_3D('',#4886,#3926,#3927);
#3405=AXIS2_PLACEMENT_3D('',#4890,#3930,#3931);
#3406=AXIS2_PLACEMENT_3D('',#4892,#3933,#3934);
#3407=AXIS2_PLACEMENT_3D('',#4896,#3937,#3938);
#3408=AXIS2_PLACEMENT_3D('',#4898,#3940,#3941);
#3409=AXIS2_PLACEMENT_3D('',#4900,#3943,#3944);
#3410=AXIS2_PLACEMENT_3D('',#4901,#3945,#3946);
#3411=AXIS2_PLACEMENT_3D('',#4902,#3947,#3948);
#3412=AXIS2_PLACEMENT_3D('',#4903,#3949,#3950);
#3413=AXIS2_PLACEMENT_3D('',#4908,#3952,#3953);
#3414=AXIS2_PLACEMENT_3D('',#4914,#3956,#3957);
#3415=AXIS2_PLACEMENT_3D('',#4916,#3959,#3960);
#3416=AXIS2_PLACEMENT_3D('',#4921,#3963,#3964);
#3417=AXIS2_PLACEMENT_3D('',#4922,#3965,#3966);
#3418=AXIS2_PLACEMENT_3D('',#4926,#3968,#3969);
#3419=AXIS2_PLACEMENT_3D('',#4928,#3971,#3972);
#3420=AXIS2_PLACEMENT_3D('',#4935,#3977,#3978);
#3421=AXIS2_PLACEMENT_3D('',#4954,#3988,#3989);
#3422=AXIS2_PLACEMENT_3D('',#4955,#3990,#3991);
#3423=AXIS2_PLACEMENT_3D('',#4970,#3999,#4000);
#3424=AXIS2_PLACEMENT_3D('',#4971,#4001,#4002);
#3425=AXIS2_PLACEMENT_3D('',#4974,#4004,#4005);
#3426=AXIS2_PLACEMENT_3D('',#4975,#4006,#4007);
#3427=AXIS2_PLACEMENT_3D('',#4978,#4009,#4010);
#3428=AXIS2_PLACEMENT_3D('',#4979,#4011,#4012);
#3429=AXIS2_PLACEMENT_3D('',#4982,#4014,#4015);
#3430=AXIS2_PLACEMENT_3D('',#4983,#4016,#4017);
#3431=AXIS2_PLACEMENT_3D('',#4985,#4018,#4019);
#3432=AXIS2_PLACEMENT_3D('',#4987,#4021,#4022);
#3433=AXIS2_PLACEMENT_3D('',#4993,#4026,#4027);
#3434=AXIS2_PLACEMENT_3D('',#4995,#4029,#4030);
#3435=AXIS2_PLACEMENT_3D('',#5005,#4036,#4037);
#3436=AXIS2_PLACEMENT_3D('',#5008,#4040,#4041);
#3437=AXIS2_PLACEMENT_3D('',#5009,#4042,#4043);
#3438=AXIS2_PLACEMENT_3D('',#5014,#4047,#4048);
#3439=AXIS2_PLACEMENT_3D('',#5018,#4051,#4052);
#3440=AXIS2_PLACEMENT_3D('',#5020,#4054,#4055);
#3441=AXIS2_PLACEMENT_3D('',#5022,#4057,#4058);
#3442=AXIS2_PLACEMENT_3D('',#5023,#4059,#4060);
#3443=AXIS2_PLACEMENT_3D('',#5024,#4061,#4062);
#3444=AXIS2_PLACEMENT_3D('',#5026,#4063,#4064);
#3445=AXIS2_PLACEMENT_3D('',#5027,#4065,#4066);
#3446=AXIS2_PLACEMENT_3D('',#5029,#4067,#4068);
#3447=AXIS2_PLACEMENT_3D('',#5042,#4075,#4076);
#3448=AXIS2_PLACEMENT_3D('',#5044,#4077,#4078);
#3449=AXIS2_PLACEMENT_3D('',#5046,#4080,#4081);
#3450=AXIS2_PLACEMENT_3D('',#5048,#4082,#4083);
#3451=AXIS2_PLACEMENT_3D('',#5050,#4085,#4086);
#3452=AXIS2_PLACEMENT_3D('',#5052,#4087,#4088);
#3453=AXIS2_PLACEMENT_3D('',#5053,#4089,#4090);
#3454=AXIS2_PLACEMENT_3D('',#5055,#4091,#4092);
#3455=AXIS2_PLACEMENT_3D('',#5057,#4094,#4095);
#3456=AXIS2_PLACEMENT_3D('',#5059,#4097,#4098);
#3457=AXIS2_PLACEMENT_3D('',#5065,#4102,#4103);
#3458=AXIS2_PLACEMENT_3D('',#5069,#4106,#4107);
#3459=AXIS2_PLACEMENT_3D('',#5073,#4110,#4111);
#3460=AXIS2_PLACEMENT_3D('',#5077,#4114,#4115);
#3461=AXIS2_PLACEMENT_3D('',#5081,#4118,#4119);
#3462=AXIS2_PLACEMENT_3D('',#5083,#4121,#4122);
#3463=AXIS2_PLACEMENT_3D('',#5084,#4123,#4124);
#3464=AXIS2_PLACEMENT_3D('',#5085,#4125,#4126);
#3465=AXIS2_PLACEMENT_3D('',#5086,#4127,#4128);
#3466=AXIS2_PLACEMENT_3D('',#5088,#4129,#4130);
#3467=AXIS2_PLACEMENT_3D('',#5091,#4132,#4133);
#3468=AXIS2_PLACEMENT_3D('',#5092,#4134,#4135);
#3469=AXIS2_PLACEMENT_3D('',#5093,#4136,#4137);
#3470=AXIS2_PLACEMENT_3D('',#5095,#4138,#4139);
#3471=AXIS2_PLACEMENT_3D('',#5097,#4141,#4142);
#3472=AXIS2_PLACEMENT_3D('',#5106,#4147,#4148);
#3473=AXIS2_PLACEMENT_3D('',#5108,#4149,#4150);
#3474=AXIS2_PLACEMENT_3D('',#5111,#4152,#4153);
#3475=AXIS2_PLACEMENT_3D('',#5112,#4154,#4155);
#3476=AXIS2_PLACEMENT_3D('',#5114,#4156,#4157);
#3477=AXIS2_PLACEMENT_3D('',#5116,#4159,#4160);
#3478=AXIS2_PLACEMENT_3D('',#5118,#4161,#4162);
#3479=AXIS2_PLACEMENT_3D('',#5120,#4164,#4165);
#3480=AXIS2_PLACEMENT_3D('',#5122,#4167,#4168);
#3481=AXIS2_PLACEMENT_3D('',#5123,#4169,#4170);
#3482=AXIS2_PLACEMENT_3D('',#5124,#4171,#4172);
#3483=AXIS2_PLACEMENT_3D('',#5127,#4173,#4174);
#3484=AXIS2_PLACEMENT_3D('',#5129,#4176,#4177);
#3485=AXIS2_PLACEMENT_3D('',#5130,#4178,#4179);
#3486=AXIS2_PLACEMENT_3D('',#5131,#4180,#4181);
#3487=AXIS2_PLACEMENT_3D('',#5133,#4182,#4183);
#3488=AXIS2_PLACEMENT_3D('',#5135,#4184,#4185);
#3489=AXIS2_PLACEMENT_3D('',#5136,#4186,#4187);
#3490=AXIS2_PLACEMENT_3D('',#5138,#4188,#4189);
#3491=AXIS2_PLACEMENT_3D('',#5139,#4190,#4191);
#3492=AXIS2_PLACEMENT_3D('',#5141,#4192,#4193);
#3493=AXIS2_PLACEMENT_3D('',#5143,#4195,#4196);
#3494=AXIS2_PLACEMENT_3D('',#5145,#4197,#4198);
#3495=AXIS2_PLACEMENT_3D('',#5147,#4200,#4201);
#3496=AXIS2_PLACEMENT_3D('',#5148,#4202,#4203);
#3497=AXIS2_PLACEMENT_3D('',#5149,#4204,#4205);
#3498=AXIS2_PLACEMENT_3D('',#5163,#4212,#4213);
#3499=AXIS2_PLACEMENT_3D('',#5164,#4214,#4215);
#3500=AXIS2_PLACEMENT_3D('',#5170,#4219,#4220);
#3501=AXIS2_PLACEMENT_3D('',#5174,#4223,#4224);
#3502=AXIS2_PLACEMENT_3D('',#5178,#4227,#4228);
#3503=AXIS2_PLACEMENT_3D('',#5182,#4231,#4232);
#3504=AXIS2_PLACEMENT_3D('',#5186,#4235,#4236);
#3505=AXIS2_PLACEMENT_3D('',#5188,#4238,#4239);
#3506=AXIS2_PLACEMENT_3D('',#5190,#4240,#4241);
#3507=AXIS2_PLACEMENT_3D('',#5193,#4243,#4244);
#3508=AXIS2_PLACEMENT_3D('',#5194,#4245,#4246);
#3509=AXIS2_PLACEMENT_3D('',#5195,#4247,#4248);
#3510=AXIS2_PLACEMENT_3D('',#5197,#4249,#4250);
#3511=AXIS2_PLACEMENT_3D('',#5199,#4252,#4253);
#3512=AXIS2_PLACEMENT_3D('',#5201,#4254,#4255);
#3513=AXIS2_PLACEMENT_3D('',#5203,#4257,#4258);
#3514=AXIS2_PLACEMENT_3D('',#5204,#4259,#4260);
#3515=AXIS2_PLACEMENT_3D('',#5206,#4261,#4262);
#3516=AXIS2_PLACEMENT_3D('',#5207,#4263,#4264);
#3517=AXIS2_PLACEMENT_3D('',#5209,#4265,#4266);
#3518=AXIS2_PLACEMENT_3D('',#5212,#4268,#4269);
#3519=AXIS2_PLACEMENT_3D('',#5213,#4270,#4271);
#3520=AXIS2_PLACEMENT_3D('',#5214,#4272,#4273);
#3521=AXIS2_PLACEMENT_3D('',#5215,#4274,#4275);
#3522=AXIS2_PLACEMENT_3D('',#5216,#4276,#4277);
#3523=AXIS2_PLACEMENT_3D('',#5217,#4278,#4279);
#3524=AXIS2_PLACEMENT_3D('',#5218,#4280,#4281);
#3525=AXIS2_PLACEMENT_3D('',#5219,#4282,#4283);
#3526=AXIS2_PLACEMENT_3D('',#5221,#4284,#4285);
#3527=AXIS2_PLACEMENT_3D('',#5224,#4287,#4288);
#3528=AXIS2_PLACEMENT_3D('',#5225,#4289,#4290);
#3529=AXIS2_PLACEMENT_3D('',#5227,#4291,#4292);
#3530=AXIS2_PLACEMENT_3D('',#5228,#4293,#4294);
#3531=AXIS2_PLACEMENT_3D('',#5230,#4295,#4296);
#3532=AXIS2_PLACEMENT_3D('',#5231,#4297,#4298);
#3533=AXIS2_PLACEMENT_3D('',#5234,#4300,#4301);
#3534=AXIS2_PLACEMENT_3D('',#5235,#4302,#4303);
#3535=AXIS2_PLACEMENT_3D('',#5247,#4305,#4306);
#3536=AXIS2_PLACEMENT_3D('',#5263,#4307,#4308);
#3537=AXIS2_PLACEMENT_3D('',#5265,#4309,#4310);
#3538=AXIS2_PLACEMENT_3D('',#5291,#4312,#4313);
#3539=AXIS2_PLACEMENT_3D('',#5294,#4316,#4317);
#3540=AXIS2_PLACEMENT_3D('',#5296,#4319,#4320);
#3541=AXIS2_PLACEMENT_3D('',#5298,#4322,#4323);
#3542=AXIS2_PLACEMENT_3D('',#5300,#4324,#4325);
#3543=AXIS2_PLACEMENT_3D('',#5302,#4327,#4328);
#3544=AXIS2_PLACEMENT_3D('',#5304,#4330,#4331);
#3545=AXIS2_PLACEMENT_3D('',#5306,#4333,#4334);
#3546=AXIS2_PLACEMENT_3D('',#5307,#4335,#4336);
#3547=AXIS2_PLACEMENT_3D('',#5308,#4337,#4338);
#3548=AXIS2_PLACEMENT_3D('',#5309,#4339,#4340);
#3549=AXIS2_PLACEMENT_3D('',#5310,#4341,#4342);
#3550=AXIS2_PLACEMENT_3D('',#5313,#4343,#4344);
#3551=AXIS2_PLACEMENT_3D('',#5315,#4345,#4346);
#3552=AXIS2_PLACEMENT_3D('',#5318,#4348,#4349);
#3553=AXIS2_PLACEMENT_3D('',#5319,#4350,#4351);
#3554=AXIS2_PLACEMENT_3D('',#5324,#4353,#4354);
#3555=AXIS2_PLACEMENT_3D('',#5326,#4355,#4356);
#3556=AXIS2_PLACEMENT_3D('',#5327,#4357,#4358);
#3557=AXIS2_PLACEMENT_3D('',#5328,#4359,#4360);
#3558=AXIS2_PLACEMENT_3D('',#5334,#4364,#4365);
#3559=AXIS2_PLACEMENT_3D('',#5340,#4369,#4370);
#3560=AXIS2_PLACEMENT_3D('',#5346,#4374,#4375);
#3561=AXIS2_PLACEMENT_3D('',#5352,#4379,#4380);
#3562=AXIS2_PLACEMENT_3D('',#5357,#4383,#4384);
#3563=AXIS2_PLACEMENT_3D('',#5358,#4385,#4386);
#3564=AXIS2_PLACEMENT_3D('',#5360,#4387,#4388);
#3565=AXIS2_PLACEMENT_3D('',#5364,#4391,#4392);
#3566=AXIS2_PLACEMENT_3D('',#5375,#4397,#4398);
#3567=AXIS2_PLACEMENT_3D('',#5377,#4400,#4401);
#3568=AXIS2_PLACEMENT_3D('',#5378,#4402,#4403);
#3569=AXIS2_PLACEMENT_3D('',#5379,#4404,#4405);
#3570=AXIS2_PLACEMENT_3D('',#5380,#4406,#4407);
#3571=AXIS2_PLACEMENT_3D('',#5381,#4408,#4409);
#3572=AXIS2_PLACEMENT_3D('',#5383,#4411,#4412);
#3573=AXIS2_PLACEMENT_3D('',#5385,#4414,#4415);
#3574=AXIS2_PLACEMENT_3D('',#5389,#4418,#4419);
#3575=AXIS2_PLACEMENT_3D('',#5393,#4422,#4423);
#3576=AXIS2_PLACEMENT_3D('',#5395,#4425,#4426);
#3577=AXIS2_PLACEMENT_3D('',#5396,#4427,#4428);
#3578=AXIS2_PLACEMENT_3D('',#5397,#4429,#4430);
#3579=AXIS2_PLACEMENT_3D('',#5399,#4431,#4432);
#3580=AXIS2_PLACEMENT_3D('',#5400,#4433,#4434);
#3581=AXIS2_PLACEMENT_3D('',#5402,#4435,#4436);
#3582=AXIS2_PLACEMENT_3D('',#5415,#4443,#4444);
#3583=AXIS2_PLACEMENT_3D('',#5417,#4445,#4446);
#3584=AXIS2_PLACEMENT_3D('',#5419,#4448,#4449);
#3585=AXIS2_PLACEMENT_3D('',#5421,#4450,#4451);
#3586=AXIS2_PLACEMENT_3D('',#5423,#4453,#4454);
#3587=AXIS2_PLACEMENT_3D('',#5425,#4455,#4456);
#3588=AXIS2_PLACEMENT_3D('',#5426,#4457,#4458);
#3589=AXIS2_PLACEMENT_3D('',#5428,#4459,#4460);
#3590=AXIS2_PLACEMENT_3D('',#5430,#4462,#4463);
#3591=AXIS2_PLACEMENT_3D('',#5432,#4465,#4466);
#3592=AXIS2_PLACEMENT_3D('',#5438,#4470,#4471);
#3593=AXIS2_PLACEMENT_3D('',#5442,#4474,#4475);
#3594=AXIS2_PLACEMENT_3D('',#5446,#4478,#4479);
#3595=AXIS2_PLACEMENT_3D('',#5450,#4482,#4483);
#3596=AXIS2_PLACEMENT_3D('',#5454,#4486,#4487);
#3597=AXIS2_PLACEMENT_3D('',#5456,#4489,#4490);
#3598=AXIS2_PLACEMENT_3D('',#5457,#4491,#4492);
#3599=AXIS2_PLACEMENT_3D('',#5458,#4493,#4494);
#3600=AXIS2_PLACEMENT_3D('',#5459,#4495,#4496);
#3601=AXIS2_PLACEMENT_3D('',#5460,#4497,#4498);
#3602=AXIS2_PLACEMENT_3D('',#5461,#4499,#4500);
#3603=AXIS2_PLACEMENT_3D('',#5462,#4501,#4502);
#3604=AXIS2_PLACEMENT_3D('',#5463,#4503,#4504);
#3605=AXIS2_PLACEMENT_3D('',#5464,#4505,#4506);
#3606=AXIS2_PLACEMENT_3D('',#5465,#4507,#4508);
#3607=AXIS2_PLACEMENT_3D('',#5466,#4509,#4510);
#3608=AXIS2_PLACEMENT_3D('',#5467,#4511,#4512);
#3609=AXIS2_PLACEMENT_3D('',#5468,#4513,#4514);
#3610=AXIS2_PLACEMENT_3D('',#5469,#4515,#4516);
#3611=AXIS2_PLACEMENT_3D('',#5470,#4517,#4518);
#3612=AXIS2_PLACEMENT_3D('',#5471,#4519,#4520);
#3613=AXIS2_PLACEMENT_3D('',#5472,#4521,#4522);
#3614=AXIS2_PLACEMENT_3D('',#5473,#4523,#4524);
#3615=AXIS2_PLACEMENT_3D('',#5474,#4525,#4526);
#3616=AXIS2_PLACEMENT_3D('',#5475,#4527,#4528);
#3617=AXIS2_PLACEMENT_3D('',#5476,#4529,#4530);
#3618=DIRECTION('axis',(0.,0.,1.));
#3619=DIRECTION('refdir',(1.,0.,0.));
#3620=DIRECTION('axis',(0.,0.,1.));
#3621=DIRECTION('refdir',(1.,0.,0.));
#3622=DIRECTION('center_axis',(0.,0.,1.));
#3623=DIRECTION('ref_axis',(1.,0.,0.));
#3624=DIRECTION('center_axis',(0.,0.,1.));
#3625=DIRECTION('ref_axis',(1.,0.,0.));
#3626=DIRECTION('',(0.,0.,1.));
#3627=DIRECTION('center_axis',(0.,0.,-1.));
#3628=DIRECTION('ref_axis',(1.,0.,0.));
#3629=DIRECTION('center_axis',(0.,0.,1.));
#3630=DIRECTION('ref_axis',(1.,0.,0.));
#3631=DIRECTION('center_axis',(0.,0.,1.));
#3632=DIRECTION('ref_axis',(1.,0.,0.));
#3633=DIRECTION('',(0.,0.,1.));
#3634=DIRECTION('center_axis',(0.,0.,-1.));
#3635=DIRECTION('ref_axis',(1.,0.,0.));
#3636=DIRECTION('center_axis',(0.,0.,1.));
#3637=DIRECTION('ref_axis',(1.,0.,0.));
#3638=DIRECTION('center_axis',(0.,0.,1.));
#3639=DIRECTION('ref_axis',(1.,0.,0.));
#3640=DIRECTION('',(0.,0.,1.));
#3641=DIRECTION('center_axis',(0.,0.,-1.));
#3642=DIRECTION('ref_axis',(1.,0.,0.));
#3643=DIRECTION('center_axis',(0.,1.,0.));
#3644=DIRECTION('ref_axis',(-1.,0.,0.));
#3645=DIRECTION('',(-1.,0.,0.));
#3646=DIRECTION('',(0.,0.,1.));
#3647=DIRECTION('',(-1.,0.,0.));
#3648=DIRECTION('',(0.,0.,1.));
#3649=DIRECTION('center_axis',(1.,0.,0.));
#3650=DIRECTION('ref_axis',(0.,1.,0.));
#3651=DIRECTION('',(0.,1.,0.));
#3652=DIRECTION('',(0.,1.,0.));
#3653=DIRECTION('',(0.,0.,1.));
#3654=DIRECTION('center_axis',(0.,-1.,0.));
#3655=DIRECTION('ref_axis',(1.,0.,0.));
#3656=DIRECTION('',(1.,0.,0.));
#3657=DIRECTION('',(1.,0.,0.));
#3658=DIRECTION('',(0.,0.,1.));
#3659=DIRECTION('center_axis',(-1.,0.,0.));
#3660=DIRECTION('ref_axis',(0.,-1.,0.));
#3661=DIRECTION('',(0.,-1.,0.));
#3662=DIRECTION('',(0.,-1.,0.));
#3663=DIRECTION('center_axis',(0.,0.,1.));
#3664=DIRECTION('ref_axis',(1.,0.,0.));
#3665=DIRECTION('center_axis',(0.,0.,1.));
#3666=DIRECTION('ref_axis',(1.,0.,0.));
#3667=DIRECTION('axis',(0.,0.,1.));
#3668=DIRECTION('refdir',(1.,0.,0.));
#3669=DIRECTION('center_axis',(0.,1.,0.));
#3670=DIRECTION('ref_axis',(1.,0.,0.));
#3671=DIRECTION('',(-1.,0.,0.));
#3672=DIRECTION('center_axis',(0.,1.,0.));
#3673=DIRECTION('ref_axis',(1.,0.,0.));
#3674=DIRECTION('',(0.,0.,1.));
#3675=DIRECTION('center_axis',(0.,1.,0.));
#3676=DIRECTION('ref_axis',(1.,0.,0.));
#3677=DIRECTION('',(-1.,0.,0.));
#3678=DIRECTION('center_axis',(0.,1.,0.));
#3679=DIRECTION('ref_axis',(1.,0.,0.));
#3680=DIRECTION('',(1.,0.,0.));
#3681=DIRECTION('',(0.,0.,-1.));
#3682=DIRECTION('center_axis',(0.,1.,0.));
#3683=DIRECTION('ref_axis',(1.,0.,0.));
#3684=DIRECTION('center_axis',(0.,-0.707106781186547,-0.707106781186548));
#3685=DIRECTION('ref_axis',(0.,0.707106781186548,-0.707106781186547));
#3686=DIRECTION('center_axis',(0.,1.,0.));
#3687=DIRECTION('ref_axis',(1.,0.,0.));
#3688=DIRECTION('',(0.,1.,0.));
#3689=DIRECTION('center_axis',(0.,0.707106781186548,0.707106781186547));
#3690=DIRECTION('ref_axis',(0.,0.707106781186547,-0.707106781186548));
#3691=DIRECTION('',(0.,1.,0.));
#3692=DIRECTION('center_axis',(0.,1.,0.));
#3693=DIRECTION('ref_axis',(1.,0.,0.));
#3694=DIRECTION('',(0.,-1.,0.));
#3695=DIRECTION('center_axis',(0.,0.707106781186547,-0.707106781186548));
#3696=DIRECTION('ref_axis',(0.,-0.707106781186548,-0.707106781186547));
#3697=DIRECTION('',(0.,-1.,0.));
#3698=DIRECTION('center_axis',(0.,-0.707106781186547,0.707106781186548));
#3699=DIRECTION('ref_axis',(0.,-0.707106781186548,-0.707106781186547));
#3700=DIRECTION('center_axis',(0.,-1.,2.77555756156289E-16));
#3701=DIRECTION('ref_axis',(1.,0.,0.));
#3702=DIRECTION('center_axis',(0.,1.,0.));
#3703=DIRECTION('ref_axis',(1.,0.,0.));
#3704=DIRECTION('',(1.,0.,0.));
#3705=DIRECTION('',(0.,0.,1.));
#3706=DIRECTION('center_axis',(0.,1.,0.));
#3707=DIRECTION('ref_axis',(1.,0.,0.));
#3708=DIRECTION('',(1.,0.,0.));
#3709=DIRECTION('',(0.,0.,-1.));
#3710=DIRECTION('',(-1.,0.,0.));
#3711=DIRECTION('center_axis',(0.,-1.,2.77555756156289E-16));
#3712=DIRECTION('ref_axis',(0.,-2.77555756156289E-16,-1.));
#3713=DIRECTION('',(1.,0.,0.));
#3714=DIRECTION('',(0.,2.77555756156289E-16,1.));
#3715=DIRECTION('',(1.,0.,0.));
#3716=DIRECTION('center_axis',(0.,-0.707106781186547,0.707106781186548));
#3717=DIRECTION('ref_axis',(0.,-0.707106781186548,-0.707106781186547));
#3718=DIRECTION('',(0.,-0.707106781186548,-0.707106781186547));
#3719=DIRECTION('',(1.,0.,0.));
#3720=DIRECTION('',(0.,0.707106781186548,0.707106781186547));
#3721=DIRECTION('center_axis',(0.,0.707106781186547,-0.707106781186548));
#3722=DIRECTION('ref_axis',(0.,0.707106781186548,0.707106781186547));
#3723=DIRECTION('',(1.,0.,0.));
#3724=DIRECTION('',(0.,-0.707106781186548,-0.707106781186547));
#3725=DIRECTION('',(1.,0.,0.));
#3726=DIRECTION('',(0.,0.707106781186548,0.707106781186547));
#3727=DIRECTION('center_axis',(0.,0.,-1.));
#3728=DIRECTION('ref_axis',(0.,1.,0.));
#3729=DIRECTION('',(0.,1.,0.));
#3730=DIRECTION('',(1.,0.,0.));
#3731=DIRECTION('',(0.,-1.,0.));
#3732=DIRECTION('center_axis',(1.,0.,0.));
#3733=DIRECTION('ref_axis',(0.,0.,-1.));
#3734=DIRECTION('',(0.,0.,1.));
#3735=DIRECTION('',(0.,-1.,0.));
#3736=DIRECTION('',(0.,0.,1.));
#3737=DIRECTION('',(0.,-1.,0.));
#3738=DIRECTION('',(0.,0.,1.));
#3739=DIRECTION('',(0.,-1.,2.41352831440251E-16));
#3740=DIRECTION('',(0.,4.44089209850063E-16,1.));
#3741=DIRECTION('',(0.,-1.,7.40148683083438E-16));
#3742=DIRECTION('center_axis',(1.,0.,0.));
#3743=DIRECTION('ref_axis',(0.,0.,-1.));
#3744=DIRECTION('',(0.,-1.,0.));
#3745=DIRECTION('',(0.,-0.707106781186548,-0.707106781186547));
#3746=DIRECTION('',(0.,0.,-1.));
#3747=DIRECTION('',(0.,1.,0.));
#3748=DIRECTION('',(0.,-2.41352831440251E-16,-1.));
#3749=DIRECTION('',(0.,1.,0.));
#3750=DIRECTION('',(0.,0.,-1.));
#3751=DIRECTION('',(0.,1.,0.));
#3752=DIRECTION('',(0.,0.,-1.));
#3753=DIRECTION('',(0.,1.,-7.40148683083438E-16));
#3754=DIRECTION('',(0.,0.707106781186547,0.707106781186548));
#3755=DIRECTION('',(0.,0.,1.));
#3756=DIRECTION('',(0.,-0.707106781186548,0.707106781186548));
#3757=DIRECTION('',(0.,-1.,0.));
#3758=DIRECTION('',(0.,0.,-1.));
#3759=DIRECTION('',(0.,-1.,0.));
#3760=DIRECTION('',(0.,0.,-1.));
#3761=DIRECTION('',(0.,-1.,0.));
#3762=DIRECTION('',(0.,0.,-1.));
#3763=DIRECTION('',(0.,-1.,0.));
#3764=DIRECTION('',(0.,0.,-1.));
#3765=DIRECTION('',(0.,0.707106781186548,-0.707106781186547));
#3766=DIRECTION('center_axis',(1.,0.,0.));
#3767=DIRECTION('ref_axis',(0.,0.,-1.));
#3768=DIRECTION('center_axis',(1.,0.,0.));
#3769=DIRECTION('ref_axis',(0.,0.,-1.));
#3770=DIRECTION('center_axis',(0.,0.,-1.));
#3771=DIRECTION('ref_axis',(0.,1.,0.));
#3772=DIRECTION('',(0.,1.,0.));
#3773=DIRECTION('',(1.,0.,0.));
#3774=DIRECTION('',(0.,-1.,0.));
#3775=DIRECTION('',(1.,0.,0.));
#3776=DIRECTION('center_axis',(0.,1.,-8.88178419700125E-16));
#3777=DIRECTION('ref_axis',(0.,8.88178419700125E-16,1.));
#3778=DIRECTION('',(0.,8.88178419700125E-16,1.));
#3779=DIRECTION('',(1.,0.,0.));
#3780=DIRECTION('',(0.,-8.88178419700125E-16,-1.));
#3781=DIRECTION('center_axis',(0.,-7.40148683083439E-16,-1.));
#3782=DIRECTION('ref_axis',(0.,1.,-7.40148683083439E-16));
#3783=DIRECTION('',(0.,1.,-7.40148683083439E-16));
#3784=DIRECTION('',(1.,0.,0.));
#3785=DIRECTION('',(0.,-1.,7.40148683083439E-16));
#3786=DIRECTION('center_axis',(0.,-0.707106781186547,-0.707106781186548));
#3787=DIRECTION('ref_axis',(0.,0.707106781186548,-0.707106781186547));
#3788=DIRECTION('',(0.,-0.707106781186548,0.707106781186547));
#3789=DIRECTION('',(0.,0.707106781186548,-0.707106781186547));
#3790=DIRECTION('center_axis',(0.,7.40148683083438E-16,1.));
#3791=DIRECTION('ref_axis',(0.,-1.,7.40148683083438E-16));
#3792=DIRECTION('',(1.,0.,0.));
#3793=DIRECTION('',(0.,1.,-7.40148683083438E-16));
#3794=DIRECTION('center_axis',(0.,1.,-4.44089209850063E-16));
#3795=DIRECTION('ref_axis',(0.,4.44089209850063E-16,1.));
#3796=DIRECTION('',(1.,0.,0.));
#3797=DIRECTION('',(0.,-4.44089209850063E-16,-1.));
#3798=DIRECTION('center_axis',(0.,2.41352831440251E-16,1.));
#3799=DIRECTION('ref_axis',(0.,-1.,2.41352831440251E-16));
#3800=DIRECTION('',(-1.,0.,0.));
#3801=DIRECTION('',(0.,1.,-2.41352831440251E-16));
#3802=DIRECTION('center_axis',(0.,-1.,2.41352831440251E-16));
#3803=DIRECTION('ref_axis',(0.,-2.41352831440251E-16,-1.));
#3804=DIRECTION('',(1.,0.,0.));
#3805=DIRECTION('',(0.,2.41352831440251E-16,1.));
#3806=DIRECTION('',(1.,0.,0.));
#3807=DIRECTION('center_axis',(0.,0.,-1.));
#3808=DIRECTION('ref_axis',(0.,1.,0.));
#3809=DIRECTION('',(1.,0.,0.));
#3810=DIRECTION('',(0.,-1.,0.));
#3811=DIRECTION('center_axis',(0.,-1.,0.));
#3812=DIRECTION('ref_axis',(0.,0.,-1.));
#3813=DIRECTION('',(1.,0.,0.));
#3814=DIRECTION('',(0.,0.,1.));
#3815=DIRECTION('center_axis',(0.,-0.707106781186547,0.707106781186548));
#3816=DIRECTION('ref_axis',(0.,-0.707106781186548,-0.707106781186547));
#3817=DIRECTION('',(1.,0.,0.));
#3818=DIRECTION('',(0.,0.707106781186548,0.707106781186547));
#3819=DIRECTION('center_axis',(0.,0.,1.));
#3820=DIRECTION('ref_axis',(0.,-1.,0.));
#3821=DIRECTION('',(1.,0.,0.));
#3822=DIRECTION('',(0.,1.,0.));
#3823=DIRECTION('center_axis',(0.,0.707106781186548,0.707106781186547));
#3824=DIRECTION('ref_axis',(0.,-0.707106781186547,0.707106781186548));
#3825=DIRECTION('',(0.,-0.707106781186547,0.707106781186548));
#3826=DIRECTION('',(1.,0.,0.));
#3827=DIRECTION('',(0.,0.707106781186547,-0.707106781186548));
#3828=DIRECTION('center_axis',(0.,1.,0.));
#3829=DIRECTION('ref_axis',(0.,0.,1.));
#3830=DIRECTION('',(0.,0.,1.));
#3831=DIRECTION('',(1.,0.,0.));
#3832=DIRECTION('',(0.,0.,-1.));
#3833=DIRECTION('center_axis',(0.,0.,-1.));
#3834=DIRECTION('ref_axis',(0.,1.,0.));
#3835=DIRECTION('',(0.,1.,0.));
#3836=DIRECTION('',(1.,0.,0.));
#3837=DIRECTION('',(0.,-1.,0.));
#3838=DIRECTION('center_axis',(0.,1.,-2.41352831440251E-16));
#3839=DIRECTION('ref_axis',(0.,2.41352831440251E-16,1.));
#3840=DIRECTION('',(0.,2.41352831440251E-16,1.));
#3841=DIRECTION('',(-1.,0.,0.));
#3842=DIRECTION('',(0.,-2.41352831440251E-16,-1.));
#3843=DIRECTION('center_axis',(0.,0.,1.));
#3844=DIRECTION('ref_axis',(0.,-1.,0.));
#3845=DIRECTION('',(1.,0.,0.));
#3846=DIRECTION('',(0.,1.,0.));
#3847=DIRECTION('',(1.,0.,0.));
#3848=DIRECTION('center_axis',(0.,-1.,0.));
#3849=DIRECTION('ref_axis',(0.,0.,-1.));
#3850=DIRECTION('',(1.,0.,0.));
#3851=DIRECTION('',(0.,0.,1.));
#3852=DIRECTION('center_axis',(0.,0.,1.));
#3853=DIRECTION('ref_axis',(0.,-1.,0.));
#3854=DIRECTION('',(1.,0.,0.));
#3855=DIRECTION('',(0.,1.,0.));
#3856=DIRECTION('center_axis',(0.,0.707106781186548,0.707106781186548));
#3857=DIRECTION('ref_axis',(0.,-0.707106781186548,0.707106781186548));
#3858=DIRECTION('',(1.,0.,0.));
#3859=DIRECTION('',(0.,0.707106781186548,-0.707106781186548));
#3860=DIRECTION('center_axis',(0.,1.,0.));
#3861=DIRECTION('ref_axis',(0.,0.,1.));
#3862=DIRECTION('',(1.,0.,0.));
#3863=DIRECTION('',(0.,0.,-1.));
#3864=DIRECTION('center_axis',(0.,0.707106781186548,-0.707106781186547));
#3865=DIRECTION('ref_axis',(0.,0.707106781186547,0.707106781186548));
#3866=DIRECTION('',(1.,0.,0.));
#3867=DIRECTION('',(0.,-0.707106781186547,-0.707106781186548));
#3868=DIRECTION('center_axis',(0.,-7.40148683083438E-16,-1.));
#3869=DIRECTION('ref_axis',(0.,1.,-7.40148683083438E-16));
#3870=DIRECTION('',(1.,0.,0.));
#3871=DIRECTION('',(0.,-1.,7.40148683083438E-16));
#3872=DIRECTION('center_axis',(0.,-1.,0.));
#3873=DIRECTION('ref_axis',(0.,0.,-1.));
#3874=DIRECTION('',(1.,0.,0.));
#3875=DIRECTION('',(0.,0.,1.));
#3876=DIRECTION('center_axis',(0.,0.,-1.));
#3877=DIRECTION('ref_axis',(0.,1.,0.));
#3878=DIRECTION('',(-1.,0.,0.));
#3879=DIRECTION('',(0.,-1.,0.));
#3880=DIRECTION('center_axis',(0.,1.,0.));
#3881=DIRECTION('ref_axis',(0.,0.,1.));
#3882=DIRECTION('',(1.,0.,0.));
#3883=DIRECTION('',(0.,0.,-1.));
#3884=DIRECTION('',(1.,0.,0.));
#3885=DIRECTION('center_axis',(0.,0.,1.));
#3886=DIRECTION('ref_axis',(0.,-1.,0.));
#3887=DIRECTION('',(1.,0.,0.));
#3888=DIRECTION('',(0.,1.,0.));
#3889=DIRECTION('center_axis',(0.,1.,0.));
#3890=DIRECTION('ref_axis',(0.,0.,1.));
#3891=DIRECTION('',(0.,0.,-1.));
#3892=DIRECTION('center_axis',(0.,-0.707106781186547,-0.707106781186548));
#3893=DIRECTION('ref_axis',(0.,0.707106781186548,-0.707106781186547));
#3894=DIRECTION('',(1.,0.,0.));
#3895=DIRECTION('',(0.,-0.707106781186548,0.707106781186547));
#3896=DIRECTION('center_axis',(0.,-1.,0.));
#3897=DIRECTION('ref_axis',(0.,0.,-1.));
#3898=DIRECTION('',(1.,0.,0.));
#3899=DIRECTION('',(0.,0.,1.));
#3900=DIRECTION('center_axis',(0.,0.,1.));
#3901=DIRECTION('ref_axis',(0.,-1.,0.));
#3902=DIRECTION('',(1.,0.,0.));
#3903=DIRECTION('',(0.,1.,0.));
#3904=DIRECTION('center_axis',(0.,-1.,0.));
#3905=DIRECTION('ref_axis',(0.,0.,-1.));
#3906=DIRECTION('',(-1.,0.,0.));
#3907=DIRECTION('',(0.,0.,1.));
#3908=DIRECTION('center_axis',(1.,0.,0.));
#3909=DIRECTION('ref_axis',(0.,0.,-1.));
#3910=DIRECTION('',(1.,0.,0.));
#3911=DIRECTION('center_axis',(-1.,0.,0.));
#3912=DIRECTION('ref_axis',(0.,0.,-1.));
#3913=DIRECTION('center_axis',(0.,1.,0.));
#3914=DIRECTION('ref_axis',(0.,0.,1.));
#3915=DIRECTION('',(1.,0.,0.));
#3916=DIRECTION('',(0.,0.,1.));
#3917=DIRECTION('center_axis',(0.,1.,0.));
#3918=DIRECTION('ref_axis',(0.,0.,1.));
#3919=DIRECTION('',(0.,0.,1.));
#3920=DIRECTION('',(1.,0.,0.));
#3921=DIRECTION('',(0.,0.,1.));
#3922=DIRECTION('center_axis',(0.,0.,-1.));
#3923=DIRECTION('ref_axis',(0.,1.,0.));
#3924=DIRECTION('',(0.,1.,0.));
#3925=DIRECTION('',(0.,1.,0.));
#3926=DIRECTION('center_axis',(0.,0.,-1.));
#3927=DIRECTION('ref_axis',(0.,1.,0.));
#3928=DIRECTION('',(0.,1.,0.));
#3929=DIRECTION('',(1.,0.,0.));
#3930=DIRECTION('center_axis',(0.,-1.,0.));
#3931=DIRECTION('ref_axis',(0.,0.,-1.));
#3932=DIRECTION('',(0.,0.,-1.));
#3933=DIRECTION('center_axis',(0.,-1.,0.));
#3934=DIRECTION('ref_axis',(0.,0.,-1.));
#3935=DIRECTION('',(0.,0.,-1.));
#3936=DIRECTION('',(1.,0.,0.));
#3937=DIRECTION('center_axis',(0.,0.,1.));
#3938=DIRECTION('ref_axis',(0.,-1.,0.));
#3939=DIRECTION('',(0.,-1.,0.));
#3940=DIRECTION('center_axis',(0.,0.,1.));
#3941=DIRECTION('ref_axis',(0.,-1.,0.));
#3942=DIRECTION('',(0.,-1.,0.));
#3943=DIRECTION('center_axis',(1.,0.,0.));
#3944=DIRECTION('ref_axis',(0.,0.,-1.));
#3945=DIRECTION('center_axis',(1.,0.,0.));
#3946=DIRECTION('ref_axis',(0.,0.,-1.));
#3947=DIRECTION('axis',(0.,0.,1.));
#3948=DIRECTION('refdir',(1.,0.,0.));
#3949=DIRECTION('center_axis',(0.,1.,0.));
#3950=DIRECTION('ref_axis',(1.,0.,0.));
#3951=DIRECTION('',(-1.,0.,0.));
#3952=DIRECTION('center_axis',(0.,1.,0.));
#3953=DIRECTION('ref_axis',(1.,0.,0.));
#3954=DIRECTION('',(1.,0.,0.));
#3955=DIRECTION('',(0.,0.,-1.));
#3956=DIRECTION('center_axis',(0.,1.,0.));
#3957=DIRECTION('ref_axis',(1.,0.,0.));
#3958=DIRECTION('',(0.,0.,1.));
#3959=DIRECTION('center_axis',(0.,1.,0.));
#3960=DIRECTION('ref_axis',(1.,0.,0.));
#3961=DIRECTION('',(0.,1.,0.));
#3962=DIRECTION('',(0.,-1.,0.));
#3963=DIRECTION('center_axis',(0.,1.,0.));
#3964=DIRECTION('ref_axis',(1.,0.,0.));
#3965=DIRECTION('center_axis',(0.,1.,0.));
#3966=DIRECTION('ref_axis',(1.,0.,0.));
#3967=DIRECTION('',(0.,-1.,0.));
#3968=DIRECTION('center_axis',(0.,1.,0.));
#3969=DIRECTION('ref_axis',(1.,0.,0.));
#3970=DIRECTION('',(0.,1.,0.));
#3971=DIRECTION('center_axis',(0.,1.,0.));
#3972=DIRECTION('ref_axis',(1.,0.,0.));
#3973=DIRECTION('',(1.,0.,0.));
#3974=DIRECTION('',(0.,0.,-1.));
#3975=DIRECTION('',(0.,0.,1.));
#3976=DIRECTION('',(-1.,0.,0.));
#3977=DIRECTION('center_axis',(0.,0.,1.));
#3978=DIRECTION('ref_axis',(1.,0.,0.));
#3979=DIRECTION('',(0.,1.,0.));
#3980=DIRECTION('',(1.,0.,0.));
#3981=DIRECTION('',(0.,-1.,0.));
#3982=DIRECTION('',(-1.,0.,0.));
#3983=DIRECTION('',(0.,1.,0.));
#3984=DIRECTION('',(1.,0.,0.));
#3985=DIRECTION('',(0.,-1.,0.));
#3986=DIRECTION('',(-1.,0.,0.));
#3987=DIRECTION('',(0.,1.,0.));
#3988=DIRECTION('center_axis',(0.,0.,-1.));
#3989=DIRECTION('ref_axis',(1.,0.,0.));
#3990=DIRECTION('center_axis',(-1.,0.,0.));
#3991=DIRECTION('ref_axis',(0.,0.,1.));
#3992=DIRECTION('',(0.,1.,0.));
#3993=DIRECTION('',(0.,0.,1.));
#3994=DIRECTION('',(0.,-1.,0.));
#3995=DIRECTION('',(0.,0.,-1.));
#3996=DIRECTION('',(0.,-1.,0.));
#3997=DIRECTION('',(0.,0.,1.));
#3998=DIRECTION('',(0.,1.,0.));
#3999=DIRECTION('center_axis',(1.,0.,0.));
#4000=DIRECTION('ref_axis',(0.,0.,-1.));
#4001=DIRECTION('center_axis',(0.,1.,0.));
#4002=DIRECTION('ref_axis',(1.,0.,0.));
#4003=DIRECTION('',(-1.,0.,0.));
#4004=DIRECTION('center_axis',(0.,1.,0.));
#4005=DIRECTION('ref_axis',(1.,0.,0.));
#4006=DIRECTION('center_axis',(0.,1.,0.));
#4007=DIRECTION('ref_axis',(1.,0.,0.));
#4008=DIRECTION('',(0.,1.,0.));
#4009=DIRECTION('center_axis',(0.,1.,0.));
#4010=DIRECTION('ref_axis',(1.,0.,0.));
#4011=DIRECTION('center_axis',(1.,0.,0.));
#4012=DIRECTION('ref_axis',(0.,0.,-1.));
#4013=DIRECTION('',(1.,0.,0.));
#4014=DIRECTION('center_axis',(-1.,0.,0.));
#4015=DIRECTION('ref_axis',(0.,0.,-1.));
#4016=DIRECTION('center_axis',(0.,0.,1.));
#4017=DIRECTION('ref_axis',(1.,0.,0.));
#4018=DIRECTION('center_axis',(0.,0.,1.));
#4019=DIRECTION('ref_axis',(1.,0.,0.));
#4020=DIRECTION('',(0.,0.,1.));
#4021=DIRECTION('center_axis',(0.707106781186548,0.,0.707106781186548));
#4022=DIRECTION('ref_axis',(0.707106781186548,0.,-0.707106781186548));
#4023=DIRECTION('',(0.707106781186548,0.,-0.707106781186548));
#4024=DIRECTION('',(0.,1.,0.));
#4025=DIRECTION('',(-0.707106781186548,0.,0.707106781186548));
#4026=DIRECTION('center_axis',(0.,1.,0.));
#4027=DIRECTION('ref_axis',(1.,0.,0.));
#4028=DIRECTION('',(0.,0.,1.));
#4029=DIRECTION('center_axis',(1.,0.,0.));
#4030=DIRECTION('ref_axis',(0.,0.,-1.));
#4031=DIRECTION('',(0.,0.,-1.));
#4032=DIRECTION('',(0.,1.,0.));
#4033=DIRECTION('',(0.,0.,1.));
#4034=DIRECTION('',(0.,1.,0.));
#4035=DIRECTION('',(0.,0.,-1.));
#4036=DIRECTION('center_axis',(0.707106781186548,0.,0.707106781186548));
#4037=DIRECTION('ref_axis',(-0.707106781186548,0.,0.707106781186548));
#4038=DIRECTION('',(-0.707106781186548,0.,0.707106781186548));
#4039=DIRECTION('',(-0.707106781186548,0.,0.707106781186548));
#4040=DIRECTION('center_axis',(0.,1.,0.));
#4041=DIRECTION('ref_axis',(1.,0.,0.));
#4042=DIRECTION('center_axis',(0.,-1.,0.));
#4043=DIRECTION('ref_axis',(0.,0.,-1.));
#4044=DIRECTION('',(1.,0.,0.));
#4045=DIRECTION('',(0.,0.,1.));
#4046=DIRECTION('',(-1.,0.,0.));
#4047=DIRECTION('center_axis',(0.,0.,-1.));
#4048=DIRECTION('ref_axis',(-1.,0.,0.));
#4049=DIRECTION('',(-1.,0.,0.));
#4050=DIRECTION('',(0.,1.,0.));
#4051=DIRECTION('center_axis',(1.,0.,0.));
#4052=DIRECTION('ref_axis',(0.,0.,-1.));
#4053=DIRECTION('',(0.,0.,-1.));
#4054=DIRECTION('center_axis',(0.,0.,1.));
#4055=DIRECTION('ref_axis',(1.,0.,0.));
#4056=DIRECTION('',(1.,0.,0.));
#4057=DIRECTION('center_axis',(0.,1.,0.));
#4058=DIRECTION('ref_axis',(0.,0.,1.));
#4059=DIRECTION('axis',(0.,0.,1.));
#4060=DIRECTION('refdir',(1.,0.,0.));
#4061=DIRECTION('center_axis',(0.,1.,0.));
#4062=DIRECTION('ref_axis',(1.,0.,0.));
#4063=DIRECTION('center_axis',(0.,-1.,0.));
#4064=DIRECTION('ref_axis',(1.,0.,0.));
#4065=DIRECTION('center_axis',(0.,1.,0.));
#4066=DIRECTION('ref_axis',(1.,0.,0.));
#4067=DIRECTION('center_axis',(0.,1.,0.));
#4068=DIRECTION('ref_axis',(1.,0.,0.));
#4069=DIRECTION('',(0.5,0.,0.866025403784439));
#4070=DIRECTION('',(1.,0.,1.20185167898973E-16));
#4071=DIRECTION('',(0.5,0.,-0.866025403784439));
#4072=DIRECTION('',(-0.5,0.,-0.866025403784439));
#4073=DIRECTION('',(-1.,0.,-2.40370335797945E-16));
#4074=DIRECTION('',(-0.5,0.,0.866025403784439));
#4075=DIRECTION('center_axis',(0.,-1.,0.));
#4076=DIRECTION('ref_axis',(1.,0.,0.));
#4077=DIRECTION('center_axis',(0.,-1.,0.));
#4078=DIRECTION('ref_axis',(1.,0.,0.));
#4079=DIRECTION('',(0.,1.,0.));
#4080=DIRECTION('center_axis',(0.,1.,0.));
#4081=DIRECTION('ref_axis',(1.,0.,0.));
#4082=DIRECTION('center_axis',(0.,-1.,0.));
#4083=DIRECTION('ref_axis',(1.,0.,0.));
#4084=DIRECTION('',(-0.707106781186547,0.707106781186548,-8.65956056235493E-17));
#4085=DIRECTION('center_axis',(0.,-1.,0.));
#4086=DIRECTION('ref_axis',(0.,0.,-1.));
#4087=DIRECTION('center_axis',(0.,-1.,0.));
#4088=DIRECTION('ref_axis',(1.,0.,0.));
#4089=DIRECTION('center_axis',(0.,1.,0.));
#4090=DIRECTION('ref_axis',(1.,0.,0.));
#4091=DIRECTION('center_axis',(0.,1.,0.));
#4092=DIRECTION('ref_axis',(1.,0.,0.));
#4093=DIRECTION('',(-0.447213595499958,0.894427190999916,-5.47678698264203E-17));
#4094=DIRECTION('center_axis',(0.,-1.,0.));
#4095=DIRECTION('ref_axis',(1.,0.,0.));
#4096=DIRECTION('',(0.,1.,0.));
#4097=DIRECTION('center_axis',(0.866025403784439,0.,-0.5));
#4098=DIRECTION('ref_axis',(0.5,0.,0.866025403784439));
#4099=DIRECTION('',(-0.5,0.,-0.866025403784439));
#4100=DIRECTION('',(0.,-1.,0.));
#4101=DIRECTION('',(0.,-1.,0.));
#4102=DIRECTION('center_axis',(1.20185167898973E-16,0.,-1.));
#4103=DIRECTION('ref_axis',(1.,0.,1.20185167898973E-16));
#4104=DIRECTION('',(-1.,0.,-1.20185167898973E-16));
#4105=DIRECTION('',(0.,-1.,0.));
#4106=DIRECTION('center_axis',(-0.866025403784439,0.,-0.5));
#4107=DIRECTION('ref_axis',(0.5,0.,-0.866025403784439));
#4108=DIRECTION('',(-0.5,0.,0.866025403784439));
#4109=DIRECTION('',(0.,-1.,0.));
#4110=DIRECTION('center_axis',(-0.866025403784439,0.,0.5));
#4111=DIRECTION('ref_axis',(-0.5,0.,-0.866025403784439));
#4112=DIRECTION('',(0.5,0.,0.866025403784439));
#4113=DIRECTION('',(0.,-1.,0.));
#4114=DIRECTION('center_axis',(-2.40370335797945E-16,0.,1.));
#4115=DIRECTION('ref_axis',(-1.,0.,-2.40370335797945E-16));
#4116=DIRECTION('',(1.,0.,2.40370335797945E-16));
#4117=DIRECTION('',(0.,-1.,0.));
#4118=DIRECTION('center_axis',(0.866025403784439,0.,0.5));
#4119=DIRECTION('ref_axis',(-0.5,0.,0.866025403784439));
#4120=DIRECTION('',(0.5,0.,-0.866025403784439));
#4121=DIRECTION('center_axis',(0.,1.,0.));
#4122=DIRECTION('ref_axis',(1.,0.,0.));
#4123=DIRECTION('axis',(0.,0.,1.));
#4124=DIRECTION('refdir',(1.,0.,0.));
#4125=DIRECTION('axis',(0.,0.,1.));
#4126=DIRECTION('refdir',(1.,0.,0.));
#4127=DIRECTION('center_axis',(0.,0.,1.));
#4128=DIRECTION('ref_axis',(1.,0.,0.));
#4129=DIRECTION('center_axis',(0.,0.,1.));
#4130=DIRECTION('ref_axis',(1.,0.,0.));
#4131=DIRECTION('',(-0.707106781186547,8.65956056235493E-17,0.707106781186548));
#4132=DIRECTION('center_axis',(0.,0.,-1.));
#4133=DIRECTION('ref_axis',(1.,0.,0.));
#4134=DIRECTION('center_axis',(0.,0.,-1.));
#4135=DIRECTION('ref_axis',(-1.,0.,0.));
#4136=DIRECTION('center_axis',(0.,0.,1.));
#4137=DIRECTION('ref_axis',(1.,0.,0.));
#4138=DIRECTION('center_axis',(0.,0.,1.));
#4139=DIRECTION('ref_axis',(1.,0.,0.));
#4140=DIRECTION('',(0.,0.,-1.));
#4141=DIRECTION('center_axis',(0.,0.,-1.));
#4142=DIRECTION('ref_axis',(1.,0.,0.));
#4143=DIRECTION('',(1.,0.,0.));
#4144=DIRECTION('',(0.,1.,0.));
#4145=DIRECTION('',(-1.,0.,0.));
#4146=DIRECTION('',(0.,-1.,0.));
#4147=DIRECTION('center_axis',(0.,1.,0.));
#4148=DIRECTION('ref_axis',(1.,0.,0.));
#4149=DIRECTION('center_axis',(0.,1.,0.));
#4150=DIRECTION('ref_axis',(1.,0.,0.));
#4151=DIRECTION('',(-1.,0.,0.));
#4152=DIRECTION('center_axis',(0.,1.,0.));
#4153=DIRECTION('ref_axis',(1.,0.,0.));
#4154=DIRECTION('center_axis',(0.,1.,0.));
#4155=DIRECTION('ref_axis',(1.,0.,0.));
#4156=DIRECTION('center_axis',(0.,1.,0.));
#4157=DIRECTION('ref_axis',(1.,0.,0.));
#4158=DIRECTION('',(0.,1.,0.));
#4159=DIRECTION('center_axis',(0.,1.,0.));
#4160=DIRECTION('ref_axis',(1.,0.,0.));
#4161=DIRECTION('center_axis',(0.,1.,0.));
#4162=DIRECTION('ref_axis',(1.,0.,0.));
#4163=DIRECTION('',(1.,0.,0.));
#4164=DIRECTION('center_axis',(0.,1.,0.));
#4165=DIRECTION('ref_axis',(1.,0.,0.));
#4166=DIRECTION('',(0.,-1.,0.));
#4167=DIRECTION('center_axis',(0.,0.,1.));
#4168=DIRECTION('ref_axis',(1.,0.,0.));
#4169=DIRECTION('axis',(0.,0.,1.));
#4170=DIRECTION('refdir',(1.,0.,0.));
#4171=DIRECTION('center_axis',(0.,-1.,0.));
#4172=DIRECTION('ref_axis',(1.,0.,0.));
#4173=DIRECTION('center_axis',(0.,1.,0.));
#4174=DIRECTION('ref_axis',(0.,0.,1.));
#4175=DIRECTION('',(1.,0.,0.));
#4176=DIRECTION('center_axis',(0.,0.,1.));
#4177=DIRECTION('ref_axis',(1.,0.,0.));
#4178=DIRECTION('center_axis',(0.,0.,-1.));
#4179=DIRECTION('ref_axis',(0.,1.,0.));
#4180=DIRECTION('center_axis',(6.12323399573676E-17,0.,1.));
#4181=DIRECTION('ref_axis',(1.,0.,0.));
#4182=DIRECTION('center_axis',(0.,0.,-1.));
#4183=DIRECTION('ref_axis',(0.,1.,0.));
#4184=DIRECTION('center_axis',(-1.22464679914735E-16,1.,0.));
#4185=DIRECTION('ref_axis',(-1.,-1.22464679914735E-16,0.));
#4186=DIRECTION('center_axis',(0.,0.,-1.));
#4187=DIRECTION('ref_axis',(-1.,0.,0.));
#4188=DIRECTION('center_axis',(0.,0.,1.));
#4189=DIRECTION('ref_axis',(1.,0.,0.));
#4190=DIRECTION('center_axis',(0.,0.,1.));
#4191=DIRECTION('ref_axis',(1.,0.,0.));
#4192=DIRECTION('center_axis',(0.,0.,1.));
#4193=DIRECTION('ref_axis',(1.,0.,0.));
#4194=DIRECTION('',(0.,0.,-1.));
#4195=DIRECTION('center_axis',(0.,0.,-1.));
#4196=DIRECTION('ref_axis',(1.,0.,0.));
#4197=DIRECTION('center_axis',(0.,0.,1.));
#4198=DIRECTION('ref_axis',(1.,0.,0.));
#4199=DIRECTION('',(-0.957826285221151,-1.17299889433528E-16,-0.287347885566345));
#4200=DIRECTION('center_axis',(0.,0.,1.));
#4201=DIRECTION('ref_axis',(1.,0.,0.));
#4202=DIRECTION('axis',(0.,0.,1.));
#4203=DIRECTION('refdir',(1.,0.,0.));
#4204=DIRECTION('center_axis',(0.,0.,1.));
#4205=DIRECTION('ref_axis',(1.,0.,0.));
#4206=DIRECTION('',(0.5,0.866025403784439,0.));
#4207=DIRECTION('',(-0.5,0.866025403784439,0.));
#4208=DIRECTION('',(-1.,1.4792020664489E-16,0.));
#4209=DIRECTION('',(-0.5,-0.866025403784439,0.));
#4210=DIRECTION('',(0.5,-0.866025403784439,0.));
#4211=DIRECTION('',(1.,-2.95840413289779E-16,0.));
#4212=DIRECTION('center_axis',(0.,0.,-1.));
#4213=DIRECTION('ref_axis',(1.,0.,0.));
#4214=DIRECTION('center_axis',(-2.95840413289779E-16,-1.,0.));
#4215=DIRECTION('ref_axis',(1.,-2.95840413289779E-16,0.));
#4216=DIRECTION('',(1.,-2.95840413289779E-16,0.));
#4217=DIRECTION('',(0.,0.,1.));
#4218=DIRECTION('',(0.,0.,1.));
#4219=DIRECTION('center_axis',(-0.866025403784439,-0.5,0.));
#4220=DIRECTION('ref_axis',(0.5,-0.866025403784439,0.));
#4221=DIRECTION('',(0.5,-0.866025403784439,0.));
#4222=DIRECTION('',(0.,0.,1.));
#4223=DIRECTION('center_axis',(-0.866025403784439,0.5,0.));
#4224=DIRECTION('ref_axis',(-0.5,-0.866025403784439,0.));
#4225=DIRECTION('',(-0.5,-0.866025403784439,0.));
#4226=DIRECTION('',(0.,0.,1.));
#4227=DIRECTION('center_axis',(1.4792020664489E-16,1.,0.));
#4228=DIRECTION('ref_axis',(-1.,1.4792020664489E-16,0.));
#4229=DIRECTION('',(-1.,1.4792020664489E-16,0.));
#4230=DIRECTION('',(0.,0.,1.));
#4231=DIRECTION('center_axis',(0.866025403784439,0.5,0.));
#4232=DIRECTION('ref_axis',(-0.5,0.866025403784439,0.));
#4233=DIRECTION('',(-0.5,0.866025403784439,0.));
#4234=DIRECTION('',(0.,0.,1.));
#4235=DIRECTION('center_axis',(0.866025403784439,-0.5,0.));
#4236=DIRECTION('ref_axis',(0.5,0.866025403784439,0.));
#4237=DIRECTION('',(0.5,0.866025403784439,0.));
#4238=DIRECTION('center_axis',(0.,0.,1.));
#4239=DIRECTION('ref_axis',(1.,0.,0.));
#4240=DIRECTION('center_axis',(0.,0.,1.));
#4241=DIRECTION('ref_axis',(1.,0.,0.));
#4242=DIRECTION('',(0.,0.,-1.));
#4243=DIRECTION('center_axis',(0.,0.,-1.));
#4244=DIRECTION('ref_axis',(1.,0.,0.));
#4245=DIRECTION('center_axis',(0.,0.,-1.));
#4246=DIRECTION('ref_axis',(-1.,0.,0.));
#4247=DIRECTION('center_axis',(0.,0.,1.));
#4248=DIRECTION('ref_axis',(1.,0.,0.));
#4249=DIRECTION('center_axis',(0.,0.,-1.));
#4250=DIRECTION('ref_axis',(1.,0.,0.));
#4251=DIRECTION('',(0.,0.,-1.));
#4252=DIRECTION('center_axis',(0.,0.,-1.));
#4253=DIRECTION('ref_axis',(1.,0.,0.));
#4254=DIRECTION('center_axis',(0.,0.,1.));
#4255=DIRECTION('ref_axis',(1.,0.,0.));
#4256=DIRECTION('',(-0.707106781186549,-8.65956056235495E-17,-0.707106781186546));
#4257=DIRECTION('center_axis',(0.,0.,1.));
#4258=DIRECTION('ref_axis',(1.,0.,0.));
#4259=DIRECTION('center_axis',(6.12323399573677E-17,0.,1.));
#4260=DIRECTION('ref_axis',(1.,0.,0.));
#4261=DIRECTION('center_axis',(1.22464679914735E-16,-1.,0.));
#4262=DIRECTION('ref_axis',(-1.,-1.22464679914735E-16,0.));
#4263=DIRECTION('center_axis',(0.,0.,1.));
#4264=DIRECTION('ref_axis',(1.,0.,0.));
#4265=DIRECTION('center_axis',(0.,0.,1.));
#4266=DIRECTION('ref_axis',(1.,0.,0.));
#4267=DIRECTION('',(0.,0.,1.));
#4268=DIRECTION('center_axis',(0.,0.,1.));
#4269=DIRECTION('ref_axis',(1.,0.,0.));
#4270=DIRECTION('center_axis',(0.,0.,1.));
#4271=DIRECTION('ref_axis',(1.,0.,0.));
#4272=DIRECTION('center_axis',(0.,0.,1.));
#4273=DIRECTION('ref_axis',(1.,0.,0.));
#4274=DIRECTION('',(0.,0.,1.));
#4275=DIRECTION('',(1.,0.,0.));
#4276=DIRECTION('',(0.,0.,1.));
#4277=DIRECTION('',(1.,0.,0.));
#4278=DIRECTION('',(0.,0.,1.));
#4279=DIRECTION('',(1.,0.,0.));
#4280=DIRECTION('axis',(0.,0.,1.));
#4281=DIRECTION('refdir',(1.,0.,0.));
#4282=DIRECTION('center_axis',(0.,1.,0.));
#4283=DIRECTION('ref_axis',(1.,0.,0.));
#4284=DIRECTION('center_axis',(0.,1.,0.));
#4285=DIRECTION('ref_axis',(1.,0.,0.));
#4286=DIRECTION('',(0.,1.,0.));
#4287=DIRECTION('center_axis',(0.,1.,0.));
#4288=DIRECTION('ref_axis',(1.,0.,0.));
#4289=DIRECTION('center_axis',(0.,1.,0.));
#4290=DIRECTION('ref_axis',(1.,0.,0.));
#4291=DIRECTION('center_axis',(0.,-1.,0.));
#4292=DIRECTION('ref_axis',(1.,0.,0.));
#4293=DIRECTION('center_axis',(0.,1.,0.));
#4294=DIRECTION('ref_axis',(1.,0.,0.));
#4295=DIRECTION('center_axis',(0.,1.,0.));
#4296=DIRECTION('ref_axis',(1.,0.,0.));
#4297=DIRECTION('center_axis',(0.,1.,0.));
#4298=DIRECTION('ref_axis',(1.,0.,0.));
#4299=DIRECTION('',(0.,-1.,0.));
#4300=DIRECTION('center_axis',(0.,1.,0.));
#4301=DIRECTION('ref_axis',(1.,0.,0.));
#4302=DIRECTION('center_axis',(0.,1.,0.));
#4303=DIRECTION('ref_axis',(1.,0.,0.));
#4304=DIRECTION('',(0.866025403784439,-0.5,1.06057523872491E-16));
#4305=DIRECTION('center_axis',(0.,-1.,0.));
#4306=DIRECTION('ref_axis',(1.,0.,0.));
#4307=DIRECTION('center_axis',(0.,-1.,0.));
#4308=DIRECTION('ref_axis',(1.,0.,0.));
#4309=DIRECTION('center_axis',(0.,1.,0.));
#4310=DIRECTION('ref_axis',(1.,0.,0.));
#4311=DIRECTION('',(-0.866025403784439,-0.5,-1.06057523872491E-16));
#4312=DIRECTION('center_axis',(1.4792020664489E-16,0.,-1.));
#4313=DIRECTION('ref_axis',(-1.,0.,-1.4792020664489E-16));
#4314=DIRECTION('',(0.,1.,0.));
#4315=DIRECTION('',(0.,1.,0.));
#4316=DIRECTION('center_axis',(-0.866025403784439,0.,-0.5));
#4317=DIRECTION('ref_axis',(-0.5,0.,0.866025403784439));
#4318=DIRECTION('',(0.,1.,0.));
#4319=DIRECTION('center_axis',(-0.866025403784439,0.,0.5));
#4320=DIRECTION('ref_axis',(0.5,0.,0.866025403784439));
#4321=DIRECTION('',(0.,1.,0.));
#4322=DIRECTION('center_axis',(0.,1.,0.));
#4323=DIRECTION('ref_axis',(1.,0.,0.));
#4324=DIRECTION('center_axis',(0.,1.,0.));
#4325=DIRECTION('ref_axis',(1.,0.,0.));
#4326=DIRECTION('',(0.,-1.,0.));
#4327=DIRECTION('center_axis',(-2.95840413289779E-16,0.,1.));
#4328=DIRECTION('ref_axis',(1.,0.,2.95840413289779E-16));
#4329=DIRECTION('',(0.,1.,0.));
#4330=DIRECTION('center_axis',(0.866025403784439,0.,-0.5));
#4331=DIRECTION('ref_axis',(-0.5,0.,-0.866025403784439));
#4332=DIRECTION('',(0.,1.,0.));
#4333=DIRECTION('center_axis',(0.866025403784439,0.,0.5));
#4334=DIRECTION('ref_axis',(0.5,0.,-0.866025403784439));
#4335=DIRECTION('center_axis',(0.,1.,0.));
#4336=DIRECTION('ref_axis',(1.,0.,0.));
#4337=DIRECTION('center_axis',(0.,1.,0.));
#4338=DIRECTION('ref_axis',(1.,0.,0.));
#4339=DIRECTION('axis',(0.,0.,1.));
#4340=DIRECTION('refdir',(1.,0.,0.));
#4341=DIRECTION('center_axis',(0.,1.,0.));
#4342=DIRECTION('ref_axis',(1.,0.,0.));
#4343=DIRECTION('center_axis',(0.,-0.707106781186548,0.707106781186548));
#4344=DIRECTION('ref_axis',(0.,-0.707106781186547,-0.707106781186547));
#4345=DIRECTION('center_axis',(0.,1.,0.));
#4346=DIRECTION('ref_axis',(1.,0.,0.));
#4347=DIRECTION('',(0.,-1.,0.));
#4348=DIRECTION('center_axis',(0.,-1.,0.));
#4349=DIRECTION('ref_axis',(1.,0.,0.));
#4350=DIRECTION('center_axis',(0.,1.,0.));
#4351=DIRECTION('ref_axis',(1.,0.,0.));
#4352=DIRECTION('',(0.,1.,0.));
#4353=DIRECTION('center_axis',(0.,1.,0.));
#4354=DIRECTION('ref_axis',(1.,0.,0.));
#4355=DIRECTION('center_axis',(0.,-0.707106781186548,0.707106781186548));
#4356=DIRECTION('ref_axis',(0.,-0.707106781186547,-0.707106781186547));
#4357=DIRECTION('center_axis',(0.,-1.,0.));
#4358=DIRECTION('ref_axis',(1.,0.,0.));
#4359=DIRECTION('center_axis',(0.,1.,0.));
#4360=DIRECTION('ref_axis',(1.,0.,0.));
#4361=DIRECTION('',(1.,0.,0.));
#4362=DIRECTION('',(0.,0.,-1.));
#4363=DIRECTION('',(-1.,0.,0.));
#4364=DIRECTION('center_axis',(0.,1.,0.));
#4365=DIRECTION('ref_axis',(1.,0.,0.));
#4366=DIRECTION('',(-1.,0.,0.));
#4367=DIRECTION('',(0.,0.,1.));
#4368=DIRECTION('',(1.,0.,0.));
#4369=DIRECTION('center_axis',(0.,1.,0.));
#4370=DIRECTION('ref_axis',(-1.,0.,0.));
#4371=DIRECTION('',(-1.,0.,0.));
#4372=DIRECTION('',(0.,0.,1.));
#4373=DIRECTION('',(1.,0.,0.));
#4374=DIRECTION('center_axis',(0.,1.,0.));
#4375=DIRECTION('ref_axis',(-1.,0.,0.));
#4376=DIRECTION('',(1.,0.,0.));
#4377=DIRECTION('',(0.,0.,1.));
#4378=DIRECTION('',(-1.,0.,0.));
#4379=DIRECTION('center_axis',(0.,0.707106781186548,-0.707106781186548));
#4380=DIRECTION('ref_axis',(-1.,0.,0.));
#4381=DIRECTION('',(0.,-0.707106781186548,-0.707106781186548));
#4382=DIRECTION('',(-1.,0.,0.));
#4383=DIRECTION('center_axis',(0.,-0.707106781186548,0.707106781186548));
#4384=DIRECTION('ref_axis',(0.,0.707106781186547,0.707106781186547));
#4385=DIRECTION('center_axis',(0.,0.707106781186548,-0.707106781186548));
#4386=DIRECTION('ref_axis',(-1.,0.,0.));
#4387=DIRECTION('center_axis',(0.,-0.707106781186548,0.707106781186548));
#4388=DIRECTION('ref_axis',(0.,0.707106781186547,0.707106781186547));
#4389=DIRECTION('',(-1.,0.,0.));
#4390=DIRECTION('',(0.,0.707106781186548,0.707106781186548));
#4391=DIRECTION('center_axis',(0.,-0.707106781186548,-0.707106781186548));
#4392=DIRECTION('ref_axis',(-1.,0.,0.));
#4393=DIRECTION('',(0.,-0.707106781186548,0.707106781186548));
#4394=DIRECTION('',(-1.,0.,0.));
#4395=DIRECTION('',(0.,0.707106781186548,-0.707106781186548));
#4396=DIRECTION('',(1.,0.,0.));
#4397=DIRECTION('center_axis',(0.,0.707106781186548,0.707106781186548));
#4398=DIRECTION('ref_axis',(0.,0.707106781186547,-0.707106781186547));
#4399=DIRECTION('',(1.,0.,0.));
#4400=DIRECTION('center_axis',(0.,0.,1.));
#4401=DIRECTION('ref_axis',(-1.83697019872103E-16,-1.,0.));
#4402=DIRECTION('center_axis',(0.,0.,-1.));
#4403=DIRECTION('ref_axis',(1.,0.,0.));
#4404=DIRECTION('center_axis',(0.,0.,-1.));
#4405=DIRECTION('ref_axis',(1.,0.,0.));
#4406=DIRECTION('center_axis',(0.,0.,-1.));
#4407=DIRECTION('ref_axis',(1.,0.,0.));
#4408=DIRECTION('center_axis',(0.,0.,1.));
#4409=DIRECTION('ref_axis',(1.,0.,0.));
#4410=DIRECTION('',(0.,-1.,0.));
#4411=DIRECTION('center_axis',(0.,0.,1.));
#4412=DIRECTION('ref_axis',(1.,0.,0.));
#4413=DIRECTION('',(0.,1.,0.));
#4414=DIRECTION('center_axis',(1.,0.,0.));
#4415=DIRECTION('ref_axis',(0.,1.,0.));
#4416=DIRECTION('',(0.,1.,0.));
#4417=DIRECTION('',(0.,0.,1.));
#4418=DIRECTION('center_axis',(0.,-1.,0.));
#4419=DIRECTION('ref_axis',(1.,0.,0.));
#4420=DIRECTION('',(1.,0.,0.));
#4421=DIRECTION('',(0.,0.,1.));
#4422=DIRECTION('center_axis',(-1.,0.,0.));
#4423=DIRECTION('ref_axis',(0.,-1.,0.));
#4424=DIRECTION('',(0.,-1.,0.));
#4425=DIRECTION('center_axis',(0.,0.,1.));
#4426=DIRECTION('ref_axis',(1.,0.,0.));
#4427=DIRECTION('axis',(0.,0.,1.));
#4428=DIRECTION('refdir',(1.,0.,0.));
#4429=DIRECTION('center_axis',(0.,1.,0.));
#4430=DIRECTION('ref_axis',(1.,0.,0.));
#4431=DIRECTION('center_axis',(0.,-1.,0.));
#4432=DIRECTION('ref_axis',(1.,0.,0.));
#4433=DIRECTION('center_axis',(0.,1.,0.));
#4434=DIRECTION('ref_axis',(1.,0.,0.));
#4435=DIRECTION('center_axis',(0.,1.,0.));
#4436=DIRECTION('ref_axis',(1.,0.,0.));
#4437=DIRECTION('',(0.5,0.,0.866025403784439));
#4438=DIRECTION('',(1.,0.,1.20185167898973E-16));
#4439=DIRECTION('',(0.5,0.,-0.866025403784439));
#4440=DIRECTION('',(-0.5,0.,-0.866025403784439));
#4441=DIRECTION('',(-1.,0.,-2.40370335797945E-16));
#4442=DIRECTION('',(-0.5,0.,0.866025403784439));
#4443=DIRECTION('center_axis',(0.,-1.,0.));
#4444=DIRECTION('ref_axis',(1.,0.,0.));
#4445=DIRECTION('center_axis',(0.,-1.,0.));
#4446=DIRECTION('ref_axis',(1.,0.,0.));
#4447=DIRECTION('',(0.,1.,0.));
#4448=DIRECTION('center_axis',(0.,1.,0.));
#4449=DIRECTION('ref_axis',(1.,0.,0.));
#4450=DIRECTION('center_axis',(0.,-1.,0.));
#4451=DIRECTION('ref_axis',(1.,0.,0.));
#4452=DIRECTION('',(-0.707106781186547,0.707106781186548,-8.65956056235493E-17));
#4453=DIRECTION('center_axis',(0.,-1.,0.));
#4454=DIRECTION('ref_axis',(0.,0.,-1.));
#4455=DIRECTION('center_axis',(0.,-1.,0.));
#4456=DIRECTION('ref_axis',(1.,0.,0.));
#4457=DIRECTION('center_axis',(0.,1.,0.));
#4458=DIRECTION('ref_axis',(1.,0.,0.));
#4459=DIRECTION('center_axis',(0.,1.,0.));
#4460=DIRECTION('ref_axis',(1.,0.,0.));
#4461=DIRECTION('',(-0.447213595499958,0.894427190999916,-5.47678698264203E-17));
#4462=DIRECTION('center_axis',(0.,-1.,0.));
#4463=DIRECTION('ref_axis',(1.,0.,0.));
#4464=DIRECTION('',(0.,1.,0.));
#4465=DIRECTION('center_axis',(0.866025403784439,0.,-0.5));
#4466=DIRECTION('ref_axis',(0.5,0.,0.866025403784439));
#4467=DIRECTION('',(-0.5,0.,-0.866025403784439));
#4468=DIRECTION('',(0.,-1.,0.));
#4469=DIRECTION('',(0.,-1.,0.));
#4470=DIRECTION('center_axis',(1.20185167898973E-16,0.,-1.));
#4471=DIRECTION('ref_axis',(1.,0.,1.20185167898973E-16));
#4472=DIRECTION('',(-1.,0.,-1.20185167898973E-16));
#4473=DIRECTION('',(0.,-1.,0.));
#4474=DIRECTION('center_axis',(-0.866025403784439,0.,-0.5));
#4475=DIRECTION('ref_axis',(0.5,0.,-0.866025403784439));
#4476=DIRECTION('',(-0.5,0.,0.866025403784439));
#4477=DIRECTION('',(0.,-1.,0.));
#4478=DIRECTION('center_axis',(-0.866025403784439,0.,0.5));
#4479=DIRECTION('ref_axis',(-0.5,0.,-0.866025403784439));
#4480=DIRECTION('',(0.5,0.,0.866025403784439));
#4481=DIRECTION('',(0.,-1.,0.));
#4482=DIRECTION('center_axis',(-2.40370335797945E-16,0.,1.));
#4483=DIRECTION('ref_axis',(-1.,0.,-2.40370335797945E-16));
#4484=DIRECTION('',(1.,0.,2.40370335797945E-16));
#4485=DIRECTION('',(0.,-1.,0.));
#4486=DIRECTION('center_axis',(0.866025403784439,0.,0.5));
#4487=DIRECTION('ref_axis',(-0.5,0.,0.866025403784439));
#4488=DIRECTION('',(0.5,0.,-0.866025403784439));
#4489=DIRECTION('center_axis',(0.,1.,0.));
#4490=DIRECTION('ref_axis',(1.,0.,0.));
#4491=DIRECTION('',(0.,0.,1.));
#4492=DIRECTION('',(1.,0.,0.));
#4493=DIRECTION('',(0.,0.,1.));
#4494=DIRECTION('',(1.,0.,0.));
#4495=DIRECTION('',(0.,0.,1.));
#4496=DIRECTION('',(2.22044604925031E-16,1.,0.));
#4497=DIRECTION('',(-1.,0.,2.22044604925031E-16));
#4498=DIRECTION('',(2.22044604925031E-16,0.,1.));
#4499=DIRECTION('',(0.,0.,1.));
#4500=DIRECTION('',(1.,0.,0.));
#4501=DIRECTION('',(0.,0.,1.));
#4502=DIRECTION('',(2.22044604925031E-16,1.,0.));
#4503=DIRECTION('',(0.,0.,1.));
#4504=DIRECTION('',(1.,0.,0.));
#4505=DIRECTION('',(0.,-1.,2.22044604925031E-16));
#4506=DIRECTION('',(1.,0.,0.));
#4507=DIRECTION('',(0.,0.,1.));
#4508=DIRECTION('',(2.22044604925031E-16,1.,0.));
#4509=DIRECTION('',(0.,-1.,2.22044604925031E-16));
#4510=DIRECTION('',(1.,0.,0.));
#4511=DIRECTION('',(1.,0.,2.22044604925031E-16));
#4512=DIRECTION('',(2.22044604925031E-16,0.,-1.));
#4513=DIRECTION('',(0.,0.,1.));
#4514=DIRECTION('',(2.22044604925031E-16,-1.,0.));
#4515=DIRECTION('',(-1.11022302462516E-16,1.,0.));
#4516=DIRECTION('',(0.,-1.11022302462516E-16,1.));
#4517=DIRECTION('',(0.,0.,1.));
#4518=DIRECTION('',(1.,0.,0.));
#4519=DIRECTION('',(0.,0.,1.));
#4520=DIRECTION('',(1.,0.,0.));
#4521=DIRECTION('',(0.,-1.,2.22044604925031E-16));
#4522=DIRECTION('',(1.,0.,0.));
#4523=DIRECTION('',(0.,-1.22464679914735E-16,-1.));
#4524=DIRECTION('',(1.,0.,0.));
#4525=DIRECTION('',(0.,1.,2.22044604925031E-16));
#4526=DIRECTION('',(1.,0.,0.));
#4527=DIRECTION('',(8.65956056235493E-17,-8.65956056235493E-17,-1.));
#4528=DIRECTION('',(2.22044604925031E-16,1.,-8.65956056235494E-17));
#4529=DIRECTION('',(0.,1.,2.22044604925031E-16));
#4530=DIRECTION('',(1.,0.,0.));
#4531=CARTESIAN_POINT('',(0.,0.,0.));
#4532=CARTESIAN_POINT('',(0.,0.,0.));
#4533=CARTESIAN_POINT('Origin',(0.,2.5,4.9));
#4534=CARTESIAN_POINT('',(-0.275,2.5,5.));
#4535=CARTESIAN_POINT('Origin',(0.,2.5,5.));
#4536=CARTESIAN_POINT('',(-0.275,2.5,6.));
#4537=CARTESIAN_POINT('',(-0.275,2.5,4.9));
#4538=CARTESIAN_POINT('Origin',(0.,2.5,6.));
#4539=CARTESIAN_POINT('Origin',(2.5,0.,4.9));
#4540=CARTESIAN_POINT('',(2.225,-3.36777869765522E-17,5.));
#4541=CARTESIAN_POINT('Origin',(2.5,0.,5.));
#4542=CARTESIAN_POINT('',(2.225,3.36777869765522E-17,6.));
#4543=CARTESIAN_POINT('',(2.225,-3.36777869765522E-17,4.9));
#4544=CARTESIAN_POINT('Origin',(2.5,0.,6.));
#4545=CARTESIAN_POINT('Origin',(0.,0.,4.9));
#4546=CARTESIAN_POINT('',(-0.34,-4.163799117101E-17,5.));
#4547=CARTESIAN_POINT('Origin',(0.,0.,5.));
#4548=CARTESIAN_POINT('',(-0.34,4.163799117101E-17,6.));
#4549=CARTESIAN_POINT('',(-0.34,-4.163799117101E-17,4.9));
#4550=CARTESIAN_POINT('Origin',(0.,0.,6.));
#4551=CARTESIAN_POINT('Origin',(3.5,3.5,5.));
#4552=CARTESIAN_POINT('',(3.5,3.5,5.));
#4553=CARTESIAN_POINT('',(-1.5,3.5,5.));
#4554=CARTESIAN_POINT('',(3.5,3.5,5.));
#4555=CARTESIAN_POINT('',(-1.5,3.5,6.));
#4556=CARTESIAN_POINT('',(-1.5,3.5,5.));
#4557=CARTESIAN_POINT('',(3.5,3.5,6.));
#4558=CARTESIAN_POINT('',(3.5,3.5,6.));
#4559=CARTESIAN_POINT('',(3.5,3.5,5.));
#4560=CARTESIAN_POINT('Origin',(3.5,-1.5,5.));
#4561=CARTESIAN_POINT('',(3.5,-1.5,5.));
#4562=CARTESIAN_POINT('',(3.5,-1.5,5.));
#4563=CARTESIAN_POINT('',(3.5,-1.5,6.));
#4564=CARTESIAN_POINT('',(3.5,-1.5,6.));
#4565=CARTESIAN_POINT('',(3.5,-1.5,5.));
#4566=CARTESIAN_POINT('Origin',(-1.5,-1.5,5.));
#4567=CARTESIAN_POINT('',(-1.5,-1.5,5.));
#4568=CARTESIAN_POINT('',(-1.5,-1.5,5.));
#4569=CARTESIAN_POINT('',(-1.5,-1.5,6.));
#4570=CARTESIAN_POINT('',(-1.5,-1.5,6.));
#4571=CARTESIAN_POINT('',(-1.5,-1.5,5.));
#4572=CARTESIAN_POINT('Origin',(-1.5,3.5,5.));
#4573=CARTESIAN_POINT('',(-1.5,3.5,5.));
#4574=CARTESIAN_POINT('',(-1.5,3.5,6.));
#4575=CARTESIAN_POINT('Origin',(1.,1.,6.));
#4576=CARTESIAN_POINT('Origin',(1.,1.,5.));
#4577=CARTESIAN_POINT('',(0.,0.,0.));
#4578=CARTESIAN_POINT('Origin',(0.,0.6,0.));
#4579=CARTESIAN_POINT('',(0.14,0.6,0.48));
#4580=CARTESIAN_POINT('',(6.93889390390723E-18,0.6,0.48));
#4581=CARTESIAN_POINT('',(-0.05,0.6,0.48));
#4582=CARTESIAN_POINT('',(0.,0.6,0.5));
#4583=CARTESIAN_POINT('Origin',(0.,0.6,0.));
#4584=CARTESIAN_POINT('',(0.,0.6,0.));
#4585=CARTESIAN_POINT('Origin',(0.,0.2,0.));
#4586=CARTESIAN_POINT('',(0.271293199325011,0.2,0.42));
#4587=CARTESIAN_POINT('',(0.,0.2,0.42));
#4588=CARTESIAN_POINT('',(-0.05,0.2,0.42));
#4589=CARTESIAN_POINT('',(0.495883050728698,0.2,0.0640312423743282));
#4590=CARTESIAN_POINT('Origin',(0.,0.2,0.));
#4591=CARTESIAN_POINT('',(0.,0.2,0.0640312423743285));
#4592=CARTESIAN_POINT('',(-0.1,0.2,0.0640312423743285));
#4593=CARTESIAN_POINT('',(0.,0.2,0.));
#4594=CARTESIAN_POINT('Origin',(0.,0.2,0.));
#4595=CARTESIAN_POINT('',(0.139999999999999,0.6,-0.48));
#4596=CARTESIAN_POINT('',(0.4,0.42,-0.3));
#4597=CARTESIAN_POINT('Origin',(0.,0.12,0.));
#4598=CARTESIAN_POINT('',(0.,0.6,-0.5));
#4599=CARTESIAN_POINT('Origin',(0.,0.6,0.));
#4600=CARTESIAN_POINT('',(0.,0.38,-0.5));
#4601=CARTESIAN_POINT('',(0.,0.2,-0.5));
#4602=CARTESIAN_POINT('',(0.271293199325011,0.3,-0.42));
#4603=CARTESIAN_POINT('Origin',(0.,-0.12,0.));
#4604=CARTESIAN_POINT('',(0.271293199325011,0.2,-0.42));
#4605=CARTESIAN_POINT('',(0.271293199325011,0.2,-0.42));
#4606=CARTESIAN_POINT('',(0.495883050728698,0.2,-0.0640312423743282));
#4607=CARTESIAN_POINT('Origin',(0.,0.2,0.));
#4608=CARTESIAN_POINT('Ctrl Pts',(0.495883050728698,0.2,0.0640312423743283));
#4609=CARTESIAN_POINT('Ctrl Pts',(0.498592889791231,0.206718816306565,0.0430451860136323));
#4610=CARTESIAN_POINT('Ctrl Pts',(0.5,0.21,0.0210250906311155));
#4611=CARTESIAN_POINT('Ctrl Pts',(0.5,0.21,-0.0210250906311155));
#4612=CARTESIAN_POINT('Ctrl Pts',(0.498592889791231,0.206718816306565,-0.0430451860136323));
#4613=CARTESIAN_POINT('Ctrl Pts',(0.495883050728698,0.2,-0.0640312423743282));
#4614=CARTESIAN_POINT('',(0.271293199325011,0.3,0.42));
#4615=CARTESIAN_POINT('',(0.271293199325011,0.2,0.42));
#4616=CARTESIAN_POINT('',(6.93889390390723E-18,0.38,0.5));
#4617=CARTESIAN_POINT('Origin',(0.,-0.12,0.));
#4618=CARTESIAN_POINT('',(0.,0.2,0.5));
#4619=CARTESIAN_POINT('',(0.4,0.42,0.3));
#4620=CARTESIAN_POINT('Origin',(0.,0.12,0.));
#4621=CARTESIAN_POINT('Origin',(0.,0.42,0.));
#4622=CARTESIAN_POINT('Origin',(0.,0.6,0.));
#4623=CARTESIAN_POINT('',(0.,0.6,-0.48));
#4624=CARTESIAN_POINT('',(-0.05,0.6,-0.48));
#4625=CARTESIAN_POINT('',(0.,0.6,0.));
#4626=CARTESIAN_POINT('Origin',(0.,0.2,0.));
#4627=CARTESIAN_POINT('',(0.,0.2,-0.42));
#4628=CARTESIAN_POINT('',(-0.05,0.2,-0.42));
#4629=CARTESIAN_POINT('',(0.,0.2,-0.0640312423743285));
#4630=CARTESIAN_POINT('',(0.,0.2,0.));
#4631=CARTESIAN_POINT('',(-0.1,0.2,-0.0640312423743285));
#4632=CARTESIAN_POINT('Origin',(-0.1,0.42,0.3));
#4633=CARTESIAN_POINT('',(10.,0.42,0.3));
#4634=CARTESIAN_POINT('',(-0.1,0.42,0.3));
#4635=CARTESIAN_POINT('',(10.,0.42,-0.3));
#4636=CARTESIAN_POINT('',(10.,0.42,0.15));
#4637=CARTESIAN_POINT('',(-0.1,0.42,-0.3));
#4638=CARTESIAN_POINT('Origin',(-0.1,0.67,0.55));
#4639=CARTESIAN_POINT('',(0.,0.67,0.55));
#4640=CARTESIAN_POINT('',(6.93889390390723E-18,0.365,0.245));
#4641=CARTESIAN_POINT('',(10.,0.67,0.55));
#4642=CARTESIAN_POINT('',(-0.1,0.67,0.55));
#4643=CARTESIAN_POINT('',(10.,0.365,0.245));
#4644=CARTESIAN_POINT('Origin',(-0.1,0.3,0.42));
#4645=CARTESIAN_POINT('',(10.,0.3,0.42));
#4646=CARTESIAN_POINT('',(-0.1,0.3,0.42));
#4647=CARTESIAN_POINT('',(10.,0.55,0.67));
#4648=CARTESIAN_POINT('',(10.,0.12,0.24));
#4649=CARTESIAN_POINT('',(0.,0.55,0.67));
#4650=CARTESIAN_POINT('',(-0.1,0.55,0.67));
#4651=CARTESIAN_POINT('',(6.93889390390723E-18,0.12,0.24));
#4652=CARTESIAN_POINT('Origin',(-0.1,-0.3,0.42));
#4653=CARTESIAN_POINT('',(0.,-0.3,0.42));
#4654=CARTESIAN_POINT('',(0.,-0.15,0.42));
#4655=CARTESIAN_POINT('',(10.,-0.3,0.42));
#4656=CARTESIAN_POINT('',(-0.1,-0.3,0.42));
#4657=CARTESIAN_POINT('',(10.,-0.15,0.42));
#4658=CARTESIAN_POINT('Origin',(0.,0.,0.));
#4659=CARTESIAN_POINT('',(0.,0.55,0.82));
#4660=CARTESIAN_POINT('',(0.,0.55,0.335));
#4661=CARTESIAN_POINT('',(0.,0.3,0.82));
#4662=CARTESIAN_POINT('',(0.,0.275,0.82));
#4663=CARTESIAN_POINT('',(0.,0.3,1.));
#4664=CARTESIAN_POINT('',(0.,0.3,0.41));
#4665=CARTESIAN_POINT('',(0.,1.,1.));
#4666=CARTESIAN_POINT('',(0.,1.,1.));
#4667=CARTESIAN_POINT('',(0.,1.,0.3));
#4668=CARTESIAN_POINT('',(0.,1.,-1.));
#4669=CARTESIAN_POINT('',(0.,0.82,0.3));
#4670=CARTESIAN_POINT('',(0.,0.525,0.3));
#4671=CARTESIAN_POINT('',(0.,0.82,0.55));
#4672=CARTESIAN_POINT('',(0.,0.82,0.15));
#4673=CARTESIAN_POINT('',(0.,0.41,0.55));
#4674=CARTESIAN_POINT('Origin',(0.,0.,0.));
#4675=CARTESIAN_POINT('',(0.,-0.3,-0.42));
#4676=CARTESIAN_POINT('',(0.,0.15,-0.42));
#4677=CARTESIAN_POINT('',(0.,-0.55,-0.67));
#4678=CARTESIAN_POINT('',(0.,-0.12,-0.24));
#4679=CARTESIAN_POINT('',(0.,-0.55,-0.82));
#4680=CARTESIAN_POINT('',(0.,-0.55,-0.335));
#4681=CARTESIAN_POINT('',(0.,-0.3,-0.82));
#4682=CARTESIAN_POINT('',(0.,-0.275,-0.82));
#4683=CARTESIAN_POINT('',(0.,-0.3,-1.));
#4684=CARTESIAN_POINT('',(0.,-0.3,-0.41));
#4685=CARTESIAN_POINT('',(0.,-1.,-1.));
#4686=CARTESIAN_POINT('',(0.,-1.,-1.));
#4687=CARTESIAN_POINT('',(0.,-1.,-0.3));
#4688=CARTESIAN_POINT('',(0.,-1.,1.));
#4689=CARTESIAN_POINT('',(0.,-0.82,-0.3));
#4690=CARTESIAN_POINT('',(0.,-0.525,-0.3));
#4691=CARTESIAN_POINT('',(0.,-0.82,-0.55));
#4692=CARTESIAN_POINT('',(0.,-0.82,-0.15));
#4693=CARTESIAN_POINT('',(0.,-0.67,-0.55));
#4694=CARTESIAN_POINT('',(0.,-0.41,-0.55));
#4695=CARTESIAN_POINT('',(0.,-0.42,-0.3));
#4696=CARTESIAN_POINT('',(0.,-0.365,-0.245));
#4697=CARTESIAN_POINT('',(0.,-0.42,0.3));
#4698=CARTESIAN_POINT('',(0.,-0.42,-0.15));
#4699=CARTESIAN_POINT('',(0.,-0.67,0.55));
#4700=CARTESIAN_POINT('',(-6.93889390390723E-18,-0.24,0.12));
#4701=CARTESIAN_POINT('',(0.,-0.82,0.55));
#4702=CARTESIAN_POINT('',(0.,-0.335,0.55));
#4703=CARTESIAN_POINT('',(0.,-0.82,0.3));
#4704=CARTESIAN_POINT('',(0.,-0.82,0.275));
#4705=CARTESIAN_POINT('',(0.,-1.,0.3));
#4706=CARTESIAN_POINT('',(0.,-0.41,0.3));
#4707=CARTESIAN_POINT('',(0.,-1.,1.));
#4708=CARTESIAN_POINT('',(0.,-1.,1.));
#4709=CARTESIAN_POINT('',(0.,-0.3,1.));
#4710=CARTESIAN_POINT('',(0.,1.,1.));
#4711=CARTESIAN_POINT('',(0.,-0.3,0.82));
#4712=CARTESIAN_POINT('',(0.,-0.3,0.525));
#4713=CARTESIAN_POINT('',(0.,-0.55,0.82));
#4714=CARTESIAN_POINT('',(0.,-0.15,0.82));
#4715=CARTESIAN_POINT('',(0.,-0.55,0.67));
#4716=CARTESIAN_POINT('',(0.,-0.55,0.41));
#4717=CARTESIAN_POINT('',(6.93889390390723E-18,-0.245,0.365));
#4718=CARTESIAN_POINT('',(0.,-2.57175827820944E-17,0.21));
#4719=CARTESIAN_POINT('Origin',(0.,0.,0.));
#4720=CARTESIAN_POINT('Origin',(0.,0.,0.));
#4721=CARTESIAN_POINT('Origin',(-0.1,0.82,-0.3));
#4722=CARTESIAN_POINT('',(0.,0.82,-0.3));
#4723=CARTESIAN_POINT('',(0.,1.,-0.3));
#4724=CARTESIAN_POINT('',(0.,0.41,-0.3));
#4725=CARTESIAN_POINT('',(10.,0.82,-0.3));
#4726=CARTESIAN_POINT('',(-0.1,0.82,-0.3));
#4727=CARTESIAN_POINT('',(10.,1.,-0.3));
#4728=CARTESIAN_POINT('',(10.,0.41,-0.3));
#4729=CARTESIAN_POINT('',(-0.05,1.,-0.3));
#4730=CARTESIAN_POINT('Origin',(-0.1,0.82,-0.55));
#4731=CARTESIAN_POINT('',(0.,0.82,-0.55));
#4732=CARTESIAN_POINT('',(0.,0.82,-0.275));
#4733=CARTESIAN_POINT('',(10.,0.82,-0.55));
#4734=CARTESIAN_POINT('',(-0.1,0.82,-0.55));
#4735=CARTESIAN_POINT('',(10.,0.82,-0.275));
#4736=CARTESIAN_POINT('Origin',(-0.1,0.67,-0.55));
#4737=CARTESIAN_POINT('',(0.,0.67,-0.55));
#4738=CARTESIAN_POINT('',(0.,0.335,-0.55));
#4739=CARTESIAN_POINT('',(10.,0.67,-0.55));
#4740=CARTESIAN_POINT('',(-0.1,0.67,-0.55));
#4741=CARTESIAN_POINT('',(10.,0.335,-0.55));
#4742=CARTESIAN_POINT('Origin',(-0.1,0.42,-0.3));
#4743=CARTESIAN_POINT('',(10.,0.24,-0.12));
#4744=CARTESIAN_POINT('',(0.,0.24,-0.12));
#4745=CARTESIAN_POINT('Origin',(-0.1,0.82,0.55));
#4746=CARTESIAN_POINT('',(10.,0.82,0.55));
#4747=CARTESIAN_POINT('',(-0.1,0.82,0.55));
#4748=CARTESIAN_POINT('',(10.,0.41,0.55));
#4749=CARTESIAN_POINT('Origin',(-0.1,0.82,0.3));
#4750=CARTESIAN_POINT('',(10.,0.82,0.3));
#4751=CARTESIAN_POINT('',(-0.1,0.82,0.3));
#4752=CARTESIAN_POINT('',(10.,0.82,0.15));
#4753=CARTESIAN_POINT('Origin',(-0.1,1.05,0.3));
#4754=CARTESIAN_POINT('',(10.,1.,0.3));
#4755=CARTESIAN_POINT('',(-0.05,1.,0.3));
#4756=CARTESIAN_POINT('',(10.,0.525,0.3));
#4757=CARTESIAN_POINT('Origin',(-0.1,-0.3,-0.82));
#4758=CARTESIAN_POINT('',(10.,-0.3,-0.82));
#4759=CARTESIAN_POINT('',(-0.1,-0.3,-0.82));
#4760=CARTESIAN_POINT('',(10.,-0.3,-1.));
#4761=CARTESIAN_POINT('',(10.,-0.3,-0.41));
#4762=CARTESIAN_POINT('',(-0.05,-0.3,-1.));
#4763=CARTESIAN_POINT('Origin',(-0.1,-0.55,-0.82));
#4764=CARTESIAN_POINT('',(10.,-0.55,-0.82));
#4765=CARTESIAN_POINT('',(-0.1,-0.55,-0.82));
#4766=CARTESIAN_POINT('',(10.,-0.275,-0.82));
#4767=CARTESIAN_POINT('Origin',(-0.1,-0.55,-0.67));
#4768=CARTESIAN_POINT('',(10.,-0.55,-0.67));
#4769=CARTESIAN_POINT('',(-0.1,-0.55,-0.67));
#4770=CARTESIAN_POINT('',(10.,-0.55,-0.335));
#4771=CARTESIAN_POINT('Origin',(-0.1,-0.3,-0.42));
#4772=CARTESIAN_POINT('',(10.,-0.3,-0.42));
#4773=CARTESIAN_POINT('',(-0.1,-0.3,-0.42));
#4774=CARTESIAN_POINT('',(10.,-0.12,-0.24));
#4775=CARTESIAN_POINT('Origin',(-0.1,0.3,-0.42));
#4776=CARTESIAN_POINT('',(10.,0.3,-0.42));
#4777=CARTESIAN_POINT('',(-0.1,0.3,-0.42));
#4778=CARTESIAN_POINT('',(10.,0.15,-0.42));
#4779=CARTESIAN_POINT('Origin',(-0.1,0.55,-0.67));
#4780=CARTESIAN_POINT('',(0.,0.55,-0.67));
#4781=CARTESIAN_POINT('',(0.,0.245,-0.365));
#4782=CARTESIAN_POINT('',(10.,0.55,-0.67));
#4783=CARTESIAN_POINT('',(-0.1,0.55,-0.67));
#4784=CARTESIAN_POINT('',(10.,0.245,-0.365));
#4785=CARTESIAN_POINT('Origin',(-0.1,0.55,-0.82));
#4786=CARTESIAN_POINT('',(0.,0.55,-0.82));
#4787=CARTESIAN_POINT('',(0.,0.55,-0.41));
#4788=CARTESIAN_POINT('',(10.,0.55,-0.82));
#4789=CARTESIAN_POINT('',(-0.1,0.55,-0.82));
#4790=CARTESIAN_POINT('',(10.,0.55,-0.41));
#4791=CARTESIAN_POINT('Origin',(-0.1,0.3,-0.82));
#4792=CARTESIAN_POINT('',(0.,0.3,-0.82));
#4793=CARTESIAN_POINT('',(0.,0.15,-0.82));
#4794=CARTESIAN_POINT('',(10.,0.3,-0.82));
#4795=CARTESIAN_POINT('',(-0.1,0.3,-0.82));
#4796=CARTESIAN_POINT('',(10.,0.15,-0.82));
#4797=CARTESIAN_POINT('Origin',(-0.1,0.3,-1.05));
#4798=CARTESIAN_POINT('',(0.,0.3,-1.));
#4799=CARTESIAN_POINT('',(0.,0.3,-0.525));
#4800=CARTESIAN_POINT('',(10.,0.3,-1.));
#4801=CARTESIAN_POINT('',(-0.05,0.3,-1.));
#4802=CARTESIAN_POINT('',(10.,0.3,-0.525));
#4803=CARTESIAN_POINT('Origin',(-0.1,-0.82,0.3));
#4804=CARTESIAN_POINT('',(10.,-0.82,0.3));
#4805=CARTESIAN_POINT('',(-0.1,-0.82,0.3));
#4806=CARTESIAN_POINT('',(10.,-1.,0.3));
#4807=CARTESIAN_POINT('',(10.,-0.41,0.3));
#4808=CARTESIAN_POINT('',(-0.05,-1.,0.3));
#4809=CARTESIAN_POINT('Origin',(-0.1,-0.82,0.55));
#4810=CARTESIAN_POINT('',(10.,-0.82,0.55));
#4811=CARTESIAN_POINT('',(-0.1,-0.82,0.55));
#4812=CARTESIAN_POINT('',(10.,-0.82,0.275));
#4813=CARTESIAN_POINT('Origin',(-0.1,-0.67,0.55));
#4814=CARTESIAN_POINT('',(10.,-0.67,0.55));
#4815=CARTESIAN_POINT('',(-0.1,-0.67,0.55));
#4816=CARTESIAN_POINT('',(10.,-0.335,0.55));
#4817=CARTESIAN_POINT('Origin',(-0.1,-0.42,0.3));
#4818=CARTESIAN_POINT('',(10.,-0.42,0.3));
#4819=CARTESIAN_POINT('',(-0.1,-0.42,0.3));
#4820=CARTESIAN_POINT('',(10.,-0.24,0.12));
#4821=CARTESIAN_POINT('Origin',(-0.1,-0.42,-0.3));
#4822=CARTESIAN_POINT('',(10.,-0.42,-0.3));
#4823=CARTESIAN_POINT('',(-0.1,-0.42,-0.3));
#4824=CARTESIAN_POINT('',(10.,-0.42,-0.15));
#4825=CARTESIAN_POINT('Origin',(-0.1,-0.67,-0.55));
#4826=CARTESIAN_POINT('',(10.,-0.67,-0.55));
#4827=CARTESIAN_POINT('',(-0.1,-0.67,-0.55));
#4828=CARTESIAN_POINT('',(10.,-0.365,-0.245));
#4829=CARTESIAN_POINT('Origin',(-0.1,-0.82,-0.55));
#4830=CARTESIAN_POINT('',(10.,-0.82,-0.55));
#4831=CARTESIAN_POINT('',(-0.1,-0.82,-0.55));
#4832=CARTESIAN_POINT('',(10.,-0.41,-0.55));
#4833=CARTESIAN_POINT('Origin',(-0.1,-0.82,-0.3));
#4834=CARTESIAN_POINT('',(10.,-0.82,-0.3));
#4835=CARTESIAN_POINT('',(-0.1,-0.82,-0.3));
#4836=CARTESIAN_POINT('',(10.,-0.82,-0.15));
#4837=CARTESIAN_POINT('Origin',(-0.1,-1.05,-0.3));
#4838=CARTESIAN_POINT('',(10.,-1.,-0.3));
#4839=CARTESIAN_POINT('',(-0.05,-1.,-0.3));
#4840=CARTESIAN_POINT('',(10.,-0.525,-0.3));
#4841=CARTESIAN_POINT('Origin',(-0.1,0.3,0.82));
#4842=CARTESIAN_POINT('',(10.,0.3,0.82));
#4843=CARTESIAN_POINT('',(-0.1,0.3,0.82));
#4844=CARTESIAN_POINT('',(10.,0.3,1.));
#4845=CARTESIAN_POINT('',(10.,0.3,0.41));
#4846=CARTESIAN_POINT('',(-0.05,0.3,1.));
#4847=CARTESIAN_POINT('Origin',(-0.1,0.55,0.82));
#4848=CARTESIAN_POINT('',(10.,0.55,0.82));
#4849=CARTESIAN_POINT('',(-0.1,0.55,0.82));
#4850=CARTESIAN_POINT('',(10.,0.275,0.82));
#4851=CARTESIAN_POINT('Origin',(-0.1,0.55,0.67));
#4852=CARTESIAN_POINT('',(10.,0.55,0.335));
#4853=CARTESIAN_POINT('Origin',(-0.1,-0.55,0.67));
#4854=CARTESIAN_POINT('',(10.,-0.55,0.67));
#4855=CARTESIAN_POINT('',(-0.1,-0.55,0.67));
#4856=CARTESIAN_POINT('',(10.,-0.245,0.365));
#4857=CARTESIAN_POINT('Origin',(-0.1,-0.55,0.82));
#4858=CARTESIAN_POINT('',(10.,-0.55,0.82));
#4859=CARTESIAN_POINT('',(-0.1,-0.55,0.82));
#4860=CARTESIAN_POINT('',(10.,-0.55,0.41));
#4861=CARTESIAN_POINT('Origin',(-0.1,-0.3,0.82));
#4862=CARTESIAN_POINT('',(10.,-0.3,0.82));
#4863=CARTESIAN_POINT('',(-0.1,-0.3,0.82));
#4864=CARTESIAN_POINT('',(10.,-0.15,0.82));
#4865=CARTESIAN_POINT('Origin',(-0.1,-0.3,1.05));
#4866=CARTESIAN_POINT('',(10.,-0.3,1.));
#4867=CARTESIAN_POINT('',(-0.05,-0.3,1.));
#4868=CARTESIAN_POINT('',(10.,-0.3,0.525));
#4869=CARTESIAN_POINT('Origin',(-0.1,0.,0.));
#4870=CARTESIAN_POINT('',(10.,2.57175827820944E-17,0.21));
#4871=CARTESIAN_POINT('',(-0.1,-2.57175827820944E-17,0.21));
#4872=CARTESIAN_POINT('Origin',(10.,0.,0.));
#4873=CARTESIAN_POINT('Origin',(0.,1.,-1.));
#4874=CARTESIAN_POINT('',(10.,1.,1.));
#4875=CARTESIAN_POINT('',(0.,1.,1.));
#4876=CARTESIAN_POINT('',(10.,1.,-1.));
#4877=CARTESIAN_POINT('Origin',(0.,1.,-1.));
#4878=CARTESIAN_POINT('',(10.,1.,-1.));
#4879=CARTESIAN_POINT('',(10.,1.,-1.));
#4880=CARTESIAN_POINT('',(0.,1.,-1.));
#4881=CARTESIAN_POINT('',(0.,1.,-1.));
#4882=CARTESIAN_POINT('',(0.,1.,-1.));
#4883=CARTESIAN_POINT('Origin',(0.,-1.,-1.));
#4884=CARTESIAN_POINT('',(0.,-1.,-1.));
#4885=CARTESIAN_POINT('',(10.,-1.,-1.));
#4886=CARTESIAN_POINT('Origin',(0.,-1.,-1.));
#4887=CARTESIAN_POINT('',(10.,-1.,-1.));
#4888=CARTESIAN_POINT('',(10.,-1.,-1.));
#4889=CARTESIAN_POINT('',(0.,-1.,-1.));
#4890=CARTESIAN_POINT('Origin',(0.,-1.,1.));
#4891=CARTESIAN_POINT('',(10.,-1.,1.));
#4892=CARTESIAN_POINT('Origin',(0.,-1.,1.));
#4893=CARTESIAN_POINT('',(10.,-1.,1.));
#4894=CARTESIAN_POINT('',(10.,-1.,1.));
#4895=CARTESIAN_POINT('',(0.,-1.,1.));
#4896=CARTESIAN_POINT('Origin',(0.,1.,1.));
#4897=CARTESIAN_POINT('',(10.,1.,1.));
#4898=CARTESIAN_POINT('Origin',(0.,1.,1.));
#4899=CARTESIAN_POINT('',(10.,1.,1.));
#4900=CARTESIAN_POINT('Origin',(10.,0.,0.));
#4901=CARTESIAN_POINT('Origin',(0.,0.,0.));
#4902=CARTESIAN_POINT('',(0.,0.,0.));
#4903=CARTESIAN_POINT('Origin',(0.,0.2,0.));
#4904=CARTESIAN_POINT('',(0.4,0.2,0.3));
#4905=CARTESIAN_POINT('',(0.3,0.2,0.3));
#4906=CARTESIAN_POINT('',(0.15,0.2,0.3));
#4907=CARTESIAN_POINT('',(0.5,0.2,0.));
#4908=CARTESIAN_POINT('Origin',(0.,0.2,0.));
#4909=CARTESIAN_POINT('',(0.,0.2,0.));
#4910=CARTESIAN_POINT('',(1.,0.2,0.));
#4911=CARTESIAN_POINT('',(0.,0.2,0.5));
#4912=CARTESIAN_POINT('',(0.,0.2,0.));
#4913=CARTESIAN_POINT('',(0.3,0.2,0.4));
#4914=CARTESIAN_POINT('Origin',(0.,0.2,0.));
#4915=CARTESIAN_POINT('',(0.3,0.2,1.));
#4916=CARTESIAN_POINT('Origin',(0.,0.2,0.));
#4917=CARTESIAN_POINT('',(0.3,0.6,0.4));
#4918=CARTESIAN_POINT('',(0.3,0.2,0.4));
#4919=CARTESIAN_POINT('',(0.,0.6,0.5));
#4920=CARTESIAN_POINT('',(0.,0.2,0.5));
#4921=CARTESIAN_POINT('Origin',(0.,0.6,0.));
#4922=CARTESIAN_POINT('Origin',(0.,0.2,0.));
#4923=CARTESIAN_POINT('',(0.4,0.6,0.3));
#4924=CARTESIAN_POINT('',(0.4,0.2,0.3));
#4925=CARTESIAN_POINT('',(0.5,0.6,0.));
#4926=CARTESIAN_POINT('Origin',(0.,0.6,0.));
#4927=CARTESIAN_POINT('',(0.5,0.2,0.));
#4928=CARTESIAN_POINT('Origin',(0.,0.6,0.));
#4929=CARTESIAN_POINT('',(0.3,0.6,0.3));
#4930=CARTESIAN_POINT('',(0.15,0.6,0.3));
#4931=CARTESIAN_POINT('',(0.3,0.6,1.));
#4932=CARTESIAN_POINT('',(0.,0.6,0.));
#4933=CARTESIAN_POINT('',(0.,0.6,0.));
#4934=CARTESIAN_POINT('',(1.,0.6,0.));
#4935=CARTESIAN_POINT('Origin',(0.3,0.,0.3));
#4936=CARTESIAN_POINT('',(0.3,-0.65,0.3));
#4937=CARTESIAN_POINT('',(0.3,0.,0.3));
#4938=CARTESIAN_POINT('',(1.849,-0.65,0.3));
#4939=CARTESIAN_POINT('',(0.68725,-0.65,0.3));
#4940=CARTESIAN_POINT('',(1.849,-0.85,0.3));
#4941=CARTESIAN_POINT('',(1.849,-0.325,0.3));
#4942=CARTESIAN_POINT('',(2.,-0.85,0.3));
#4943=CARTESIAN_POINT('',(2.,-0.85,0.3));
#4944=CARTESIAN_POINT('',(2.,0.85,0.3));
#4945=CARTESIAN_POINT('',(2.,0.,0.3));
#4946=CARTESIAN_POINT('',(1.849,0.85,0.3));
#4947=CARTESIAN_POINT('',(2.,0.85,0.3));
#4948=CARTESIAN_POINT('',(1.849,0.65,0.3));
#4949=CARTESIAN_POINT('',(1.849,0.325,0.3));
#4950=CARTESIAN_POINT('',(0.3,0.65,0.3));
#4951=CARTESIAN_POINT('',(0.68725,0.65,0.3));
#4952=CARTESIAN_POINT('',(0.3,0.,0.3));
#4953=CARTESIAN_POINT('',(0.725,3.36777869765522E-17,0.3));
#4954=CARTESIAN_POINT('Origin',(1.,0.,0.3));
#4955=CARTESIAN_POINT('Origin',(0.,0.,0.));
#4956=CARTESIAN_POINT('',(0.,-0.8,0.));
#4957=CARTESIAN_POINT('',(0.,0.,0.));
#4958=CARTESIAN_POINT('',(0.,-0.8,0.3));
#4959=CARTESIAN_POINT('',(0.,-0.8,0.));
#4960=CARTESIAN_POINT('',(0.,-0.85,0.3));
#4961=CARTESIAN_POINT('',(0.,-2.1,0.3));
#4962=CARTESIAN_POINT('',(0.,-0.85,2.));
#4963=CARTESIAN_POINT('',(0.,-0.85,2.));
#4964=CARTESIAN_POINT('',(0.,0.85,2.));
#4965=CARTESIAN_POINT('',(0.,0.,2.));
#4966=CARTESIAN_POINT('',(0.,0.85,0.));
#4967=CARTESIAN_POINT('',(0.,0.85,2.));
#4968=CARTESIAN_POINT('',(0.,0.,0.));
#4969=CARTESIAN_POINT('',(0.,-3.36777869765522E-17,1.275));
#4970=CARTESIAN_POINT('Origin',(0.,0.,1.));
#4971=CARTESIAN_POINT('Origin',(0.,-0.8,0.));
#4972=CARTESIAN_POINT('',(0.3,-0.8,0.));
#4973=CARTESIAN_POINT('',(1.,-0.8,0.));
#4974=CARTESIAN_POINT('Origin',(0.,-0.8,0.));
#4975=CARTESIAN_POINT('Origin',(0.,-2.1,0.));
#4976=CARTESIAN_POINT('',(0.3,-0.85,0.));
#4977=CARTESIAN_POINT('',(0.3,-2.1,0.));
#4978=CARTESIAN_POINT('Origin',(0.,-0.85,0.));
#4979=CARTESIAN_POINT('Origin',(-0.05,0.,1.));
#4980=CARTESIAN_POINT('',(0.3,3.36777869765522E-17,1.275));
#4981=CARTESIAN_POINT('',(-0.05,-3.36777869765522E-17,1.275));
#4982=CARTESIAN_POINT('Origin',(0.3,0.,1.));
#4983=CARTESIAN_POINT('Origin',(1.,0.,-0.05));
#4984=CARTESIAN_POINT('',(0.725,-3.36777869765522E-17,0.));
#4985=CARTESIAN_POINT('Origin',(1.,0.,0.));
#4986=CARTESIAN_POINT('',(0.725,-3.36777869765522E-17,-0.05));
#4987=CARTESIAN_POINT('Origin',(0.299,0.65,1.85));
#4988=CARTESIAN_POINT('',(0.3,0.85,1.849));
#4989=CARTESIAN_POINT('',(1.85,0.85,0.299));
#4990=CARTESIAN_POINT('',(0.3,0.65,1.849));
#4991=CARTESIAN_POINT('',(0.3,0.325,1.849));
#4992=CARTESIAN_POINT('',(1.85,0.65,0.299));
#4993=CARTESIAN_POINT('Origin',(1.0745,0.65,1.0745));
#4994=CARTESIAN_POINT('',(0.3,0.65,1.53725));
#4995=CARTESIAN_POINT('Origin',(0.3,0.,2.));
#4996=CARTESIAN_POINT('',(0.3,0.85,2.));
#4997=CARTESIAN_POINT('',(0.3,0.85,0.3));
#4998=CARTESIAN_POINT('',(0.3,-0.85,2.));
#4999=CARTESIAN_POINT('',(0.3,0.,2.));
#5000=CARTESIAN_POINT('',(0.3,-0.85,1.849));
#5001=CARTESIAN_POINT('',(0.3,-0.85,0.3));
#5002=CARTESIAN_POINT('',(0.3,-0.65,1.849));
#5003=CARTESIAN_POINT('',(0.3,-0.325,1.849));
#5004=CARTESIAN_POINT('',(0.3,-0.65,1.53725));
#5005=CARTESIAN_POINT('Origin',(1.85,-0.65,0.299));
#5006=CARTESIAN_POINT('',(1.85,-0.85,0.299));
#5007=CARTESIAN_POINT('',(1.85,-0.65,0.299));
#5008=CARTESIAN_POINT('Origin',(1.0745,-0.65,1.0745));
#5009=CARTESIAN_POINT('Origin',(1.,-0.85,1.));
#5010=CARTESIAN_POINT('',(2.,-0.85,0.));
#5011=CARTESIAN_POINT('',(0.,-0.85,0.));
#5012=CARTESIAN_POINT('',(2.,-0.85,0.));
#5013=CARTESIAN_POINT('',(0.3,-0.85,2.));
#5014=CARTESIAN_POINT('Origin',(2.,0.,0.));
#5015=CARTESIAN_POINT('',(2.,0.85,0.));
#5016=CARTESIAN_POINT('',(0.,0.85,0.));
#5017=CARTESIAN_POINT('',(2.,0.,0.));
#5018=CARTESIAN_POINT('Origin',(2.,0.,0.3));
#5019=CARTESIAN_POINT('',(2.,0.85,0.));
#5020=CARTESIAN_POINT('Origin',(0.,0.,2.));
#5021=CARTESIAN_POINT('',(0.3,0.85,2.));
#5022=CARTESIAN_POINT('Origin',(1.,0.85,1.));
#5023=CARTESIAN_POINT('',(0.,0.,0.));
#5024=CARTESIAN_POINT('Origin',(0.,0.2,0.));
#5025=CARTESIAN_POINT('',(-0.425,0.2,-5.20474889637625E-17));
#5026=CARTESIAN_POINT('Origin',(0.,0.2,0.));
#5027=CARTESIAN_POINT('Origin',(0.,-0.8,0.));
#5028=CARTESIAN_POINT('',(-0.24505,-0.8,3.00099698131059E-17));
#5029=CARTESIAN_POINT('Origin',(0.,-0.8,0.));
#5030=CARTESIAN_POINT('',(0.115470053837925,-0.8,-0.2));
#5031=CARTESIAN_POINT('',(0.23094010767585,-0.8,0.));
#5032=CARTESIAN_POINT('',(0.23094010767585,-0.8,0.));
#5033=CARTESIAN_POINT('',(-0.115470053837925,-0.8,-0.2));
#5034=CARTESIAN_POINT('',(0.115470053837925,-0.8,-0.2));
#5035=CARTESIAN_POINT('',(-0.23094010767585,-0.8,-2.77555756156289E-17));
#5036=CARTESIAN_POINT('',(-0.115470053837925,-0.8,-0.2));
#5037=CARTESIAN_POINT('',(-0.115470053837925,-0.8,0.2));
#5038=CARTESIAN_POINT('',(-0.23094010767585,-0.8,-2.82820063659975E-17));
#5039=CARTESIAN_POINT('',(0.115470053837925,-0.8,0.2));
#5040=CARTESIAN_POINT('',(-0.115470053837925,-0.8,0.2));
#5041=CARTESIAN_POINT('',(0.115470053837925,-0.8,0.2));
#5042=CARTESIAN_POINT('Origin',(0.,0.24,0.));
#5043=CARTESIAN_POINT('',(-0.425,0.0299999999999998,-5.20474889637625E-17));
#5044=CARTESIAN_POINT('Origin',(0.,0.0299999999999998,0.));
#5045=CARTESIAN_POINT('',(-0.425,0.24,-5.20474889637625E-17));
#5046=CARTESIAN_POINT('Origin',(0.,0.0150000000000001,0.));
#5047=CARTESIAN_POINT('',(-0.395,4.85722573273506E-17,-4.83735485663204E-17));
#5048=CARTESIAN_POINT('Origin',(0.,0.,0.));
#5049=CARTESIAN_POINT('',(-0.41,0.0150000000000001,-5.02105187650415E-17));
#5050=CARTESIAN_POINT('Origin',(0.27,0.,0.));
#5051=CARTESIAN_POINT('',(-0.27,0.,-3.30654635769785E-17));
#5052=CARTESIAN_POINT('Origin',(0.,0.,0.));
#5053=CARTESIAN_POINT('Origin',(0.,-0.02,0.));
#5054=CARTESIAN_POINT('',(-0.24505,-0.0498999999999999,3.00099698131059E-17));
#5055=CARTESIAN_POINT('Origin',(0.,-0.0498999999999999,0.));
#5056=CARTESIAN_POINT('',(-0.26,-0.02,-3.18408167778312E-17));
#5057=CARTESIAN_POINT('Origin',(0.,-0.995,0.));
#5058=CARTESIAN_POINT('',(-0.24505,-0.995,-3.00099698131059E-17));
#5059=CARTESIAN_POINT('Origin',(0.115470053837925,-0.5,-0.2));
#5060=CARTESIAN_POINT('',(0.23094010767585,-0.5,0.));
#5061=CARTESIAN_POINT('',(0.115470053837925,-0.5,-0.2));
#5062=CARTESIAN_POINT('',(0.23094010767585,-0.5,0.));
#5063=CARTESIAN_POINT('',(0.115470053837925,-0.5,-0.2));
#5064=CARTESIAN_POINT('',(0.23094010767585,-0.5,0.));
#5065=CARTESIAN_POINT('Origin',(-0.115470053837925,-0.5,-0.2));
#5066=CARTESIAN_POINT('',(-0.115470053837925,-0.5,-0.2));
#5067=CARTESIAN_POINT('',(0.115470053837925,-0.5,-0.2));
#5068=CARTESIAN_POINT('',(-0.115470053837925,-0.5,-0.2));
#5069=CARTESIAN_POINT('Origin',(-0.23094010767585,-0.5,-2.77555756156289E-17));
#5070=CARTESIAN_POINT('',(-0.23094010767585,-0.5,-2.82820063659975E-17));
#5071=CARTESIAN_POINT('',(-0.115470053837925,-0.5,-0.2));
#5072=CARTESIAN_POINT('',(-0.23094010767585,-0.5,-2.82820063659975E-17));
#5073=CARTESIAN_POINT('Origin',(-0.115470053837925,-0.5,0.2));
#5074=CARTESIAN_POINT('',(-0.115470053837925,-0.5,0.2));
#5075=CARTESIAN_POINT('',(-0.23094010767585,-0.5,-2.82820063659975E-17));
#5076=CARTESIAN_POINT('',(-0.115470053837925,-0.5,0.2));
#5077=CARTESIAN_POINT('Origin',(0.115470053837925,-0.5,0.2));
#5078=CARTESIAN_POINT('',(0.115470053837925,-0.5,0.2));
#5079=CARTESIAN_POINT('',(-0.115470053837925,-0.5,0.2));
#5080=CARTESIAN_POINT('',(0.115470053837925,-0.5,0.2));
#5081=CARTESIAN_POINT('Origin',(0.23094010767585,-0.5,0.));
#5082=CARTESIAN_POINT('',(0.115470053837925,-0.5,0.2));
#5083=CARTESIAN_POINT('Origin',(0.,-0.5,0.));
#5084=CARTESIAN_POINT('',(0.,0.,0.));
#5085=CARTESIAN_POINT('',(0.,0.,0.));
#5086=CARTESIAN_POINT('Origin',(0.,0.,0.1));
#5087=CARTESIAN_POINT('',(-1.8,-2.20436423846524E-16,0.));
#5088=CARTESIAN_POINT('Origin',(0.,0.,0.));
#5089=CARTESIAN_POINT('',(-2.,2.44929359829471E-16,0.2));
#5090=CARTESIAN_POINT('',(-1.9,2.32682891837997E-16,0.1));
#5091=CARTESIAN_POINT('Origin',(0.,0.,0.2));
#5092=CARTESIAN_POINT('Origin',(1.9,0.,0.));
#5093=CARTESIAN_POINT('Origin',(0.,0.,0.25));
#5094=CARTESIAN_POINT('',(-2.,-2.44929359829471E-16,0.4));
#5095=CARTESIAN_POINT('Origin',(0.,0.,0.4));
#5096=CARTESIAN_POINT('',(-2.,-2.44929359829471E-16,0.25));
#5097=CARTESIAN_POINT('Origin',(0.,0.,0.3));
#5098=CARTESIAN_POINT('',(-0.4,0.6,0.3));
#5099=CARTESIAN_POINT('',(0.4,0.6,0.3));
#5100=CARTESIAN_POINT('',(0.,0.6,0.3));
#5101=CARTESIAN_POINT('',(-0.4,0.2,0.3));
#5102=CARTESIAN_POINT('',(-0.4,0.2,0.3));
#5103=CARTESIAN_POINT('',(0.4,0.2,0.3));
#5104=CARTESIAN_POINT('',(0.,0.2,0.3));
#5105=CARTESIAN_POINT('',(0.4,0.2,0.3));
#5106=CARTESIAN_POINT('Origin',(0.,0.2,0.));
#5107=CARTESIAN_POINT('',(-0.3,0.2,0.4));
#5108=CARTESIAN_POINT('Origin',(0.,0.2,0.));
#5109=CARTESIAN_POINT('',(0.3,0.2,0.4));
#5110=CARTESIAN_POINT('',(0.,0.2,0.4));
#5111=CARTESIAN_POINT('Origin',(0.,0.2,0.));
#5112=CARTESIAN_POINT('Origin',(0.,0.2,0.));
#5113=CARTESIAN_POINT('',(-0.3,0.6,0.4));
#5114=CARTESIAN_POINT('Origin',(0.,0.6,0.));
#5115=CARTESIAN_POINT('',(-0.3,0.2,0.4));
#5116=CARTESIAN_POINT('Origin',(0.,0.6,0.));
#5117=CARTESIAN_POINT('',(0.3,0.6,0.4));
#5118=CARTESIAN_POINT('Origin',(0.,0.6,0.));
#5119=CARTESIAN_POINT('',(0.,0.6,0.4));
#5120=CARTESIAN_POINT('Origin',(0.,0.2,0.));
#5121=CARTESIAN_POINT('',(0.3,0.2,0.4));
#5122=CARTESIAN_POINT('Origin',(0.,0.,0.4));
#5123=CARTESIAN_POINT('',(0.,0.,0.));
#5124=CARTESIAN_POINT('Origin',(-0.3,0.2,0.4));
#5125=CARTESIAN_POINT('',(0.265329983228433,0.2,0.7));
#5126=CARTESIAN_POINT('',(-0.265329983228432,0.2,0.7));
#5127=CARTESIAN_POINT('Origin',(1.11022302462516E-16,0.2,1.1));
#5128=CARTESIAN_POINT('',(-0.3,0.2,0.7));
#5129=CARTESIAN_POINT('Origin',(0.,0.4,0.7));
#5130=CARTESIAN_POINT('Origin',(1.11022302462516E-16,0.,0.7));
#5131=CARTESIAN_POINT('Origin',(1.11022302462516E-16,0.,1.1));
#5132=CARTESIAN_POINT('',(-0.48,-5.8783046359073E-17,1.3));
#5133=CARTESIAN_POINT('Origin',(1.11022302462516E-16,0.,1.3));
#5134=CARTESIAN_POINT('',(7.91814856846845E-17,-3.89937543492083E-33,0.58));
#5135=CARTESIAN_POINT('Origin',(1.11022302462516E-16,0.,1.1));
#5136=CARTESIAN_POINT('Origin',(2.,0.,0.4));
#5137=CARTESIAN_POINT('',(-2.,-2.44929359829471E-16,0.4));
#5138=CARTESIAN_POINT('Origin',(0.,0.,0.4));
#5139=CARTESIAN_POINT('Origin',(0.,0.,0.7));
#5140=CARTESIAN_POINT('',(-2.,-2.44929359829471E-16,1.));
#5141=CARTESIAN_POINT('Origin',(0.,0.,1.));
#5142=CARTESIAN_POINT('',(-2.,-2.44929359829471E-16,0.7));
#5143=CARTESIAN_POINT('Origin',(0.,0.,1.15));
#5144=CARTESIAN_POINT('',(-1.,-1.22464679914735E-16,1.3));
#5145=CARTESIAN_POINT('Origin',(0.,0.,1.3));
#5146=CARTESIAN_POINT('',(-1.5,-1.83697019872103E-16,1.15));
#5147=CARTESIAN_POINT('Origin',(0.,0.,1.3));
#5148=CARTESIAN_POINT('',(0.,0.,0.));
#5149=CARTESIAN_POINT('Origin',(0.,1.11022302462516E-16,2.5));
#5150=CARTESIAN_POINT('',(0.375277674973257,-0.65,2.5));
#5151=CARTESIAN_POINT('',(0.750555349946514,0.,2.5));
#5152=CARTESIAN_POINT('',(0.375277674973257,-0.65,2.5));
#5153=CARTESIAN_POINT('',(0.375277674973257,0.65,2.5));
#5154=CARTESIAN_POINT('',(0.750555349946514,0.,2.5));
#5155=CARTESIAN_POINT('',(-0.375277674973257,0.65,2.5));
#5156=CARTESIAN_POINT('',(0.375277674973257,0.65,2.5));
#5157=CARTESIAN_POINT('',(-0.750555349946514,1.11022302462516E-16,2.5));
#5158=CARTESIAN_POINT('',(-0.375277674973257,0.65,2.5));
#5159=CARTESIAN_POINT('',(-0.375277674973257,-0.65,2.5));
#5160=CARTESIAN_POINT('',(-0.750555349946514,9.19165206894919E-17,2.5));
#5161=CARTESIAN_POINT('',(-0.375277674973257,-0.65,2.5));
#5162=CARTESIAN_POINT('',(-0.3933,4.81653586104654E-17,2.5));
#5163=CARTESIAN_POINT('Origin',(0.,0.,2.5));
#5164=CARTESIAN_POINT('Origin',(-0.375277674973257,-0.65,1.8));
#5165=CARTESIAN_POINT('',(-0.375277674973257,-0.65,1.8));
#5166=CARTESIAN_POINT('',(0.375277674973257,-0.65,1.8));
#5167=CARTESIAN_POINT('',(-0.375277674973257,-0.65,1.8));
#5168=CARTESIAN_POINT('',(0.375277674973257,-0.65,1.8));
#5169=CARTESIAN_POINT('',(-0.375277674973257,-0.65,1.8));
#5170=CARTESIAN_POINT('Origin',(-0.750555349946514,9.19165206894919E-17,
1.8));
#5171=CARTESIAN_POINT('',(-0.750555349946514,9.19165206894919E-17,1.8));
#5172=CARTESIAN_POINT('',(-0.750555349946514,9.19165206894919E-17,1.8));
#5173=CARTESIAN_POINT('',(-0.750555349946514,9.19165206894919E-17,1.8));
#5174=CARTESIAN_POINT('Origin',(-0.375277674973257,0.65,1.8));
#5175=CARTESIAN_POINT('',(-0.375277674973257,0.65,1.8));
#5176=CARTESIAN_POINT('',(-0.375277674973257,0.65,1.8));
#5177=CARTESIAN_POINT('',(-0.375277674973257,0.65,1.8));
#5178=CARTESIAN_POINT('Origin',(0.375277674973257,0.65,1.8));
#5179=CARTESIAN_POINT('',(0.375277674973257,0.65,1.8));
#5180=CARTESIAN_POINT('',(0.375277674973257,0.65,1.8));
#5181=CARTESIAN_POINT('',(0.375277674973257,0.65,1.8));
#5182=CARTESIAN_POINT('Origin',(0.750555349946514,0.,1.8));
#5183=CARTESIAN_POINT('',(0.750555349946514,0.,1.8));
#5184=CARTESIAN_POINT('',(0.750555349946514,0.,1.8));
#5185=CARTESIAN_POINT('',(0.750555349946514,0.,1.8));
#5186=CARTESIAN_POINT('Origin',(0.375277674973257,-0.65,1.8));
#5187=CARTESIAN_POINT('',(0.375277674973257,-0.65,1.8));
#5188=CARTESIAN_POINT('Origin',(0.,0.,1.45));
#5189=CARTESIAN_POINT('',(-0.3,-3.67394039744206E-17,1.8));
#5190=CARTESIAN_POINT('Origin',(0.,0.,1.8));
#5191=CARTESIAN_POINT('',(-0.3,3.67394039744206E-17,1.5));
#5192=CARTESIAN_POINT('',(-0.3,-3.67394039744206E-17,1.45));
#5193=CARTESIAN_POINT('Origin',(0.,0.,1.5));
#5194=CARTESIAN_POINT('Origin',(0.4,0.,1.8));
#5195=CARTESIAN_POINT('Origin',(0.,0.,4.6));
#5196=CARTESIAN_POINT('',(-0.3933,4.81653586104654E-17,7.4067));
#5197=CARTESIAN_POINT('Origin',(0.,0.,7.4067));
#5198=CARTESIAN_POINT('',(-0.3933,-4.81653586104654E-17,4.6));
#5199=CARTESIAN_POINT('Origin',(0.,0.,7.45));
#5200=CARTESIAN_POINT('',(-0.3,-3.67394039744206E-17,7.5));
#5201=CARTESIAN_POINT('Origin',(0.,0.,7.5));
#5202=CARTESIAN_POINT('',(-0.35,-4.28626379701574E-17,7.45));
#5203=CARTESIAN_POINT('Origin',(0.,0.,7.5));
#5204=CARTESIAN_POINT('Origin',(-5.55111512312578E-17,0.,1.1));
#5205=CARTESIAN_POINT('',(-8.61273212099417E-17,-3.74939945665464E-33,0.6));
#5206=CARTESIAN_POINT('Origin',(-5.55111512312578E-17,0.,1.1));
#5207=CARTESIAN_POINT('Origin',(0.,0.,4.9));
#5208=CARTESIAN_POINT('',(-0.34,-4.163799117101E-17,4.9));
#5209=CARTESIAN_POINT('Origin',(0.,0.,4.9));
#5210=CARTESIAN_POINT('',(-0.34,-4.163799117101E-17,6.1));
#5211=CARTESIAN_POINT('',(-0.34,-4.163799117101E-17,4.9));
#5212=CARTESIAN_POINT('Origin',(0.,0.,6.1));
#5213=CARTESIAN_POINT('Origin',(0.,0.,6.1));
#5214=CARTESIAN_POINT('Origin',(0.,0.,4.9));
#5215=CARTESIAN_POINT('',(0.,0.,0.));
#5216=CARTESIAN_POINT('',(0.,0.,0.));
#5217=CARTESIAN_POINT('',(0.,0.,0.));
#5218=CARTESIAN_POINT('',(0.,0.,0.));
#5219=CARTESIAN_POINT('Origin',(0.,0.2,0.));
#5220=CARTESIAN_POINT('',(-0.5,0.2,6.12323399573677E-17));
#5221=CARTESIAN_POINT('Origin',(0.,0.2,0.));
#5222=CARTESIAN_POINT('',(-0.5,0.6,6.12323399573677E-17));
#5223=CARTESIAN_POINT('',(-0.5,0.2,6.12323399573677E-17));
#5224=CARTESIAN_POINT('Origin',(0.,0.6,0.));
#5225=CARTESIAN_POINT('Origin',(0.,0.6,0.));
#5226=CARTESIAN_POINT('',(-0.338975,0.6,-4.15124648740974E-17));
#5227=CARTESIAN_POINT('Origin',(0.,0.6,0.));
#5228=CARTESIAN_POINT('Origin',(0.,0.2,0.));
#5229=CARTESIAN_POINT('',(-0.338975,0.2,4.15124648740974E-17));
#5230=CARTESIAN_POINT('Origin',(0.,0.2,0.));
#5231=CARTESIAN_POINT('Origin',(0.,0.,0.));
#5232=CARTESIAN_POINT('',(-0.338975,0.,4.15124648740974E-17));
#5233=CARTESIAN_POINT('',(-0.338975,0.,4.15124648740974E-17));
#5234=CARTESIAN_POINT('Origin',(0.,0.,0.));
#5235=CARTESIAN_POINT('Origin',(0.,0.067277284513851,0.));
#5236=CARTESIAN_POINT('',(-0.375277674973257,0.0768195421087395,0.65));
#5237=CARTESIAN_POINT('',(0.375277674973257,0.0768195421087395,0.65));
#5238=CARTESIAN_POINT('Ctrl Pts',(-0.375277674973257,0.0768195421087395,
0.65));
#5239=CARTESIAN_POINT('Ctrl Pts',(1.66533453693773E-13,-0.0315137912242439,
0.65));
#5240=CARTESIAN_POINT('Ctrl Pts',(0.375277674973257,0.0768195421087394,
0.65));
#5241=CARTESIAN_POINT('',(-0.750555349946514,0.0768195421087394,-9.19165206894919E-17));
#5242=CARTESIAN_POINT('Ctrl Pts',(-0.750555349946514,0.0768195421087394,
-9.19165206894919E-17));
#5243=CARTESIAN_POINT('Ctrl Pts',(-0.562916512459802,-0.0315137912242434,
0.325000000000144));
#5244=CARTESIAN_POINT('Ctrl Pts',(-0.375277674973257,0.0768195421087395,
0.65));
#5245=CARTESIAN_POINT('',(-0.6175,-2.77555756156289E-17,-7.5621939847349E-17));
#5246=CARTESIAN_POINT('',(-0.734027674973257,0.067277284513851,-8.98924642641573E-17));
#5247=CARTESIAN_POINT('Origin',(0.,0.,0.));
#5248=CARTESIAN_POINT('',(-0.375277674973257,0.0768195421087395,-0.65));
#5249=CARTESIAN_POINT('Ctrl Pts',(-0.375277674973257,0.0768195421087395,
-0.65));
#5250=CARTESIAN_POINT('Ctrl Pts',(-0.562916512459968,-0.0315137912242437,
-0.324999999999856));
#5251=CARTESIAN_POINT('Ctrl Pts',(-0.750555349946514,0.0768195421087395,
-9.19165206894919E-17));
#5252=CARTESIAN_POINT('',(0.375277674973257,0.0768195421087395,-0.65));
#5253=CARTESIAN_POINT('Ctrl Pts',(0.375277674973257,0.0768195421087395,
-0.65));
#5254=CARTESIAN_POINT('Ctrl Pts',(-1.66144875635155E-13,-0.0315137912242437,
-0.65));
#5255=CARTESIAN_POINT('Ctrl Pts',(-0.375277674973257,0.0768195421087395,
-0.65));
#5256=CARTESIAN_POINT('',(0.750555349946514,0.0768195421087394,0.));
#5257=CARTESIAN_POINT('Ctrl Pts',(0.750555349946514,0.0768195421087394,
0.));
#5258=CARTESIAN_POINT('Ctrl Pts',(0.562916512459802,-0.0315137912242436,
-0.325000000000144));
#5259=CARTESIAN_POINT('Ctrl Pts',(0.375277674973257,0.0768195421087395,
-0.65));
#5260=CARTESIAN_POINT('Ctrl Pts',(0.375277674973257,0.0768195421087394,
0.65));
#5261=CARTESIAN_POINT('Ctrl Pts',(0.562916512459968,-0.0315137912242439,
0.324999999999856));
#5262=CARTESIAN_POINT('Ctrl Pts',(0.750555349946514,0.0768195421087394,
0.));
#5263=CARTESIAN_POINT('Origin',(0.,0.612722715486149,0.));
#5264=CARTESIAN_POINT('',(-0.6175,0.68,-7.5621939847349E-17));
#5265=CARTESIAN_POINT('Origin',(0.,0.68,0.));
#5266=CARTESIAN_POINT('',(-0.750555349946514,0.603180457891261,-9.19165206894919E-17));
#5267=CARTESIAN_POINT('',(-0.734027674973257,0.612722715486149,-8.98924642641573E-17));
#5268=CARTESIAN_POINT('',(-0.375277674973257,0.603180457891261,0.65));
#5269=CARTESIAN_POINT('Ctrl Pts',(-0.375277674973257,0.603180457891261,
0.65));
#5270=CARTESIAN_POINT('Ctrl Pts',(-0.562916512459968,0.711513791224243,
0.324999999999856));
#5271=CARTESIAN_POINT('Ctrl Pts',(-0.750555349946514,0.603180457891261,
-9.19165206894919E-17));
#5272=CARTESIAN_POINT('',(0.375277674973257,0.603180457891261,0.65));
#5273=CARTESIAN_POINT('Ctrl Pts',(0.375277674973257,0.603180457891261,0.65));
#5274=CARTESIAN_POINT('Ctrl Pts',(-1.66755498298699E-13,0.711513791224244,
0.65));
#5275=CARTESIAN_POINT('Ctrl Pts',(-0.375277674973257,0.603180457891261,
0.65));
#5276=CARTESIAN_POINT('',(0.750555349946514,0.603180457891261,0.));
#5277=CARTESIAN_POINT('Ctrl Pts',(0.750555349946514,0.603180457891261,0.));
#5278=CARTESIAN_POINT('Ctrl Pts',(0.562916512459802,0.711513791224244,0.325000000000144));
#5279=CARTESIAN_POINT('Ctrl Pts',(0.375277674973257,0.603180457891261,0.65));
#5280=CARTESIAN_POINT('',(0.375277674973257,0.603180457891261,-0.65));
#5281=CARTESIAN_POINT('Ctrl Pts',(0.375277674973257,0.603180457891261,-0.65));
#5282=CARTESIAN_POINT('Ctrl Pts',(0.562916512459969,0.711513791224244,-0.324999999999856));
#5283=CARTESIAN_POINT('Ctrl Pts',(0.750555349946514,0.603180457891261,0.));
#5284=CARTESIAN_POINT('',(-0.375277674973257,0.603180457891261,-0.65));
#5285=CARTESIAN_POINT('Ctrl Pts',(-0.375277674973257,0.603180457891261,
-0.65));
#5286=CARTESIAN_POINT('Ctrl Pts',(1.66422431391311E-13,0.711513791224244,
-0.65));
#5287=CARTESIAN_POINT('Ctrl Pts',(0.375277674973257,0.603180457891261,-0.65));
#5288=CARTESIAN_POINT('Ctrl Pts',(-0.750555349946514,0.603180457891261,
-9.19165206894919E-17));
#5289=CARTESIAN_POINT('Ctrl Pts',(-0.562916512459802,0.711513791224244,
-0.325000000000144));
#5290=CARTESIAN_POINT('Ctrl Pts',(-0.375277674973257,0.603180457891261,
-0.65));
#5291=CARTESIAN_POINT('Origin',(0.375277674973257,0.,-0.65));
#5292=CARTESIAN_POINT('',(-0.375277674973257,0.,-0.65));
#5293=CARTESIAN_POINT('',(0.375277674973257,0.,-0.65));
#5294=CARTESIAN_POINT('Origin',(-0.375277674973257,0.,-0.65));
#5295=CARTESIAN_POINT('',(-0.750555349946514,0.,-9.19165206894919E-17));
#5296=CARTESIAN_POINT('Origin',(-0.750555349946514,0.,-9.19165206894919E-17));
#5297=CARTESIAN_POINT('',(-0.375277674973257,0.,0.65));
#5298=CARTESIAN_POINT('Origin',(0.,0.,0.));
#5299=CARTESIAN_POINT('',(-0.338975,0.68,4.15124648740974E-17));
#5300=CARTESIAN_POINT('Origin',(0.,0.68,0.));
#5301=CARTESIAN_POINT('',(-0.338975,0.,4.15124648740974E-17));
#5302=CARTESIAN_POINT('Origin',(-0.375277674973257,0.,0.65));
#5303=CARTESIAN_POINT('',(0.375277674973257,0.,0.65));
#5304=CARTESIAN_POINT('Origin',(0.750555349946514,0.,0.));
#5305=CARTESIAN_POINT('',(0.750555349946514,0.,0.));
#5306=CARTESIAN_POINT('Origin',(0.375277674973257,0.,0.65));
#5307=CARTESIAN_POINT('Origin',(0.,0.68,-1.11022302462516E-16));
#5308=CARTESIAN_POINT('Origin',(0.,0.,-1.11022302462516E-16));
#5309=CARTESIAN_POINT('',(0.,0.,0.));
#5310=CARTESIAN_POINT('Origin',(0.,0.2,0.));
#5311=CARTESIAN_POINT('',(0.49749371855331,0.2,0.05));
#5312=CARTESIAN_POINT('',(0.476969600708473,0.3,0.15));
#5313=CARTESIAN_POINT('Origin',(0.,0.15,0.));
#5314=CARTESIAN_POINT('',(0.3,0.2,0.4));
#5315=CARTESIAN_POINT('Origin',(0.,0.2,0.));
#5316=CARTESIAN_POINT('',(0.3,0.3,0.4));
#5317=CARTESIAN_POINT('',(0.3,0.2,0.4));
#5318=CARTESIAN_POINT('Origin',(0.,0.3,0.));
#5319=CARTESIAN_POINT('Origin',(0.,0.2,0.));
#5320=CARTESIAN_POINT('',(-0.3,0.2,0.4));
#5321=CARTESIAN_POINT('',(-0.3,0.3,0.4));
#5322=CARTESIAN_POINT('',(-0.3,0.2,0.4));
#5323=CARTESIAN_POINT('',(-0.49749371855331,0.2,0.05));
#5324=CARTESIAN_POINT('Origin',(0.,0.2,0.));
#5325=CARTESIAN_POINT('',(-0.476969600708473,0.3,0.15));
#5326=CARTESIAN_POINT('Origin',(0.,0.15,0.));
#5327=CARTESIAN_POINT('Origin',(0.,0.3,0.));
#5328=CARTESIAN_POINT('Origin',(0.,0.2,0.));
#5329=CARTESIAN_POINT('',(0.069403818338763,0.2,0.05));
#5330=CARTESIAN_POINT('',(0.125,0.2,0.05));
#5331=CARTESIAN_POINT('',(0.0694038183387628,0.2,0.4));
#5332=CARTESIAN_POINT('',(0.0694038183387628,0.2,-0.1));
#5333=CARTESIAN_POINT('',(0.,0.2,0.4));
#5334=CARTESIAN_POINT('Origin',(0.,0.2,0.));
#5335=CARTESIAN_POINT('',(-0.0694038183387628,0.2,0.4));
#5336=CARTESIAN_POINT('',(0.,0.2,0.4));
#5337=CARTESIAN_POINT('',(-0.069403818338763,0.2,0.05));
#5338=CARTESIAN_POINT('',(-0.0694038183387628,0.2,-0.1));
#5339=CARTESIAN_POINT('',(0.125,0.2,0.05));
#5340=CARTESIAN_POINT('Origin',(0.5,0.3,0.));
#5341=CARTESIAN_POINT('',(0.5,0.3,0.4));
#5342=CARTESIAN_POINT('',(0.5,0.3,0.4));
#5343=CARTESIAN_POINT('',(0.5,0.3,0.15));
#5344=CARTESIAN_POINT('',(0.5,0.3,0.));
#5345=CARTESIAN_POINT('',(0.25,0.3,0.15));
#5346=CARTESIAN_POINT('Origin',(0.5,0.3,0.));
#5347=CARTESIAN_POINT('',(-0.5,0.3,0.15));
#5348=CARTESIAN_POINT('',(0.25,0.3,0.15));
#5349=CARTESIAN_POINT('',(-0.5,0.3,0.4));
#5350=CARTESIAN_POINT('',(-0.5,0.3,0.));
#5351=CARTESIAN_POINT('',(0.5,0.3,0.4));
#5352=CARTESIAN_POINT('Origin',(0.25,0.225,0.075));
#5353=CARTESIAN_POINT('',(0.5,0.15,0.));
#5354=CARTESIAN_POINT('',(0.5,0.075,-0.075));
#5355=CARTESIAN_POINT('',(0.149388386429468,0.15,0.));
#5356=CARTESIAN_POINT('',(0.25,0.15,0.));
#5357=CARTESIAN_POINT('Origin',(0.,0.,-0.15));
#5358=CARTESIAN_POINT('Origin',(0.25,0.225,0.075));
#5359=CARTESIAN_POINT('',(-0.149388386429468,0.15,0.));
#5360=CARTESIAN_POINT('Origin',(0.,0.,-0.15));
#5361=CARTESIAN_POINT('',(-0.5,0.15,0.));
#5362=CARTESIAN_POINT('',(0.25,0.15,0.));
#5363=CARTESIAN_POINT('',(-0.5,0.225,0.075));
#5364=CARTESIAN_POINT('Origin',(-0.25,-0.225,0.075));
#5365=CARTESIAN_POINT('',(0.5,-0.15,0.));
#5366=CARTESIAN_POINT('',(0.5,-0.3,0.15));
#5367=CARTESIAN_POINT('',(0.5,-0.225,0.075));
#5368=CARTESIAN_POINT('',(-0.5,-0.3,0.15));
#5369=CARTESIAN_POINT('',(-0.25,-0.3,0.15));
#5370=CARTESIAN_POINT('',(-0.5,-0.15,0.));
#5371=CARTESIAN_POINT('',(-0.5,-0.075,-0.075));
#5372=CARTESIAN_POINT('',(-0.149388386429468,-0.15,0.));
#5373=CARTESIAN_POINT('',(-0.25,-0.15,0.));
#5374=CARTESIAN_POINT('',(0.149388386429468,-0.15,0.));
#5375=CARTESIAN_POINT('Origin',(0.,0.,-0.15));
#5376=CARTESIAN_POINT('',(-0.25,-0.15,0.));
#5377=CARTESIAN_POINT('Origin',(0.,0.,-0.1));
#5378=CARTESIAN_POINT('Origin',(0.,0.,0.4));
#5379=CARTESIAN_POINT('Origin',(0.,0.,0.));
#5380=CARTESIAN_POINT('Origin',(0.,0.,0.));
#5381=CARTESIAN_POINT('Origin',(0.,0.,0.));
#5382=CARTESIAN_POINT('',(-0.5,0.3,0.));
#5383=CARTESIAN_POINT('Origin',(0.,0.,0.));
#5384=CARTESIAN_POINT('',(0.5,-0.3,0.));
#5385=CARTESIAN_POINT('Origin',(0.5,-0.3,0.));
#5386=CARTESIAN_POINT('',(0.5,-0.3,0.4));
#5387=CARTESIAN_POINT('',(0.5,-0.3,0.4));
#5388=CARTESIAN_POINT('',(0.5,-0.3,0.));
#5389=CARTESIAN_POINT('Origin',(-0.5,-0.3,0.));
#5390=CARTESIAN_POINT('',(-0.5,-0.3,0.4));
#5391=CARTESIAN_POINT('',(-0.5,-0.3,0.4));
#5392=CARTESIAN_POINT('',(-0.5,-0.3,0.));
#5393=CARTESIAN_POINT('Origin',(-0.5,0.3,0.));
#5394=CARTESIAN_POINT('',(-0.5,0.3,0.4));
#5395=CARTESIAN_POINT('Origin',(0.,0.,0.4));
#5396=CARTESIAN_POINT('',(0.,0.,0.));
#5397=CARTESIAN_POINT('Origin',(0.,0.2,0.));
#5398=CARTESIAN_POINT('',(-0.425,0.2,-5.20474889637625E-17));
#5399=CARTESIAN_POINT('Origin',(0.,0.2,0.));
#5400=CARTESIAN_POINT('Origin',(0.,-0.8,0.));
#5401=CARTESIAN_POINT('',(-0.24505,-0.8,3.00099698131059E-17));
#5402=CARTESIAN_POINT('Origin',(0.,-0.8,0.));
#5403=CARTESIAN_POINT('',(0.115470053837925,-0.8,-0.2));
#5404=CARTESIAN_POINT('',(0.23094010767585,-0.8,0.));
#5405=CARTESIAN_POINT('',(0.23094010767585,-0.8,0.));
#5406=CARTESIAN_POINT('',(-0.115470053837925,-0.8,-0.2));
#5407=CARTESIAN_POINT('',(0.115470053837925,-0.8,-0.2));
#5408=CARTESIAN_POINT('',(-0.23094010767585,-0.8,-2.77555756156289E-17));
#5409=CARTESIAN_POINT('',(-0.115470053837925,-0.8,-0.2));
#5410=CARTESIAN_POINT('',(-0.115470053837925,-0.8,0.2));
#5411=CARTESIAN_POINT('',(-0.23094010767585,-0.8,-2.82820063659975E-17));
#5412=CARTESIAN_POINT('',(0.115470053837925,-0.8,0.2));
#5413=CARTESIAN_POINT('',(-0.115470053837925,-0.8,0.2));
#5414=CARTESIAN_POINT('',(0.115470053837925,-0.8,0.2));
#5415=CARTESIAN_POINT('Origin',(0.,0.24,0.));
#5416=CARTESIAN_POINT('',(-0.425,0.0299999999999998,-5.20474889637625E-17));
#5417=CARTESIAN_POINT('Origin',(0.,0.0299999999999998,0.));
#5418=CARTESIAN_POINT('',(-0.425,0.24,-5.20474889637625E-17));
#5419=CARTESIAN_POINT('Origin',(0.,0.0150000000000001,0.));
#5420=CARTESIAN_POINT('',(-0.395,4.85722573273506E-17,-4.83735485663204E-17));
#5421=CARTESIAN_POINT('Origin',(0.,0.,0.));
#5422=CARTESIAN_POINT('',(-0.41,0.0150000000000001,-5.02105187650415E-17));
#5423=CARTESIAN_POINT('Origin',(0.27,0.,0.));
#5424=CARTESIAN_POINT('',(-0.27,0.,-3.30654635769785E-17));
#5425=CARTESIAN_POINT('Origin',(0.,0.,0.));
#5426=CARTESIAN_POINT('Origin',(0.,-0.02,0.));
#5427=CARTESIAN_POINT('',(-0.24505,-0.0498999999999999,3.00099698131059E-17));
#5428=CARTESIAN_POINT('Origin',(0.,-0.0498999999999999,0.));
#5429=CARTESIAN_POINT('',(-0.26,-0.02,-3.18408167778312E-17));
#5430=CARTESIAN_POINT('Origin',(0.,-0.995,0.));
#5431=CARTESIAN_POINT('',(-0.24505,-0.995,-3.00099698131059E-17));
#5432=CARTESIAN_POINT('Origin',(0.115470053837925,-0.5,-0.2));
#5433=CARTESIAN_POINT('',(0.23094010767585,-0.5,0.));
#5434=CARTESIAN_POINT('',(0.115470053837925,-0.5,-0.2));
#5435=CARTESIAN_POINT('',(0.23094010767585,-0.5,0.));
#5436=CARTESIAN_POINT('',(0.115470053837925,-0.5,-0.2));
#5437=CARTESIAN_POINT('',(0.23094010767585,-0.5,0.));
#5438=CARTESIAN_POINT('Origin',(-0.115470053837925,-0.5,-0.2));
#5439=CARTESIAN_POINT('',(-0.115470053837925,-0.5,-0.2));
#5440=CARTESIAN_POINT('',(0.115470053837925,-0.5,-0.2));
#5441=CARTESIAN_POINT('',(-0.115470053837925,-0.5,-0.2));
#5442=CARTESIAN_POINT('Origin',(-0.23094010767585,-0.5,-2.77555756156289E-17));
#5443=CARTESIAN_POINT('',(-0.23094010767585,-0.5,-2.82820063659975E-17));
#5444=CARTESIAN_POINT('',(-0.115470053837925,-0.5,-0.2));
#5445=CARTESIAN_POINT('',(-0.23094010767585,-0.5,-2.82820063659975E-17));
#5446=CARTESIAN_POINT('Origin',(-0.115470053837925,-0.5,0.2));
#5447=CARTESIAN_POINT('',(-0.115470053837925,-0.5,0.2));
#5448=CARTESIAN_POINT('',(-0.23094010767585,-0.5,-2.82820063659975E-17));
#5449=CARTESIAN_POINT('',(-0.115470053837925,-0.5,0.2));
#5450=CARTESIAN_POINT('Origin',(0.115470053837925,-0.5,0.2));
#5451=CARTESIAN_POINT('',(0.115470053837925,-0.5,0.2));
#5452=CARTESIAN_POINT('',(-0.115470053837925,-0.5,0.2));
#5453=CARTESIAN_POINT('',(0.115470053837925,-0.5,0.2));
#5454=CARTESIAN_POINT('Origin',(0.23094010767585,-0.5,0.));
#5455=CARTESIAN_POINT('',(0.115470053837925,-0.5,0.2));
#5456=CARTESIAN_POINT('Origin',(0.,-0.5,0.));
#5457=CARTESIAN_POINT('',(0.,0.,0.));
#5458=CARTESIAN_POINT('',(1.,0.,7.));
#5459=CARTESIAN_POINT('',(0.,1.,7.));
#5460=CARTESIAN_POINT('',(0.,0.,7.6));
#5461=CARTESIAN_POINT('',(1.,0.,8.));
#5462=CARTESIAN_POINT('',(0.,1.,8.));
#5463=CARTESIAN_POINT('',(2.,0.,7.42));
#5464=CARTESIAN_POINT('',(2.,0.,8.3));
#5465=CARTESIAN_POINT('',(0.,2.,7.42));
#5466=CARTESIAN_POINT('',(0.,2.,8.3));
#5467=CARTESIAN_POINT('',(0.42,0.,9.));
#5468=CARTESIAN_POINT('',(1.3,0.,9.));
#5469=CARTESIAN_POINT('',(0.,0.42,9.));
#5470=CARTESIAN_POINT('',(0.,1.3,9.));
#5471=CARTESIAN_POINT('',(0.,0.,0.));
#5472=CARTESIAN_POINT('',(0.,0.,6.));
#5473=CARTESIAN_POINT('',(2.5,0.,6.58));
#5474=CARTESIAN_POINT('',(2.5,0.,5.));
#5475=CARTESIAN_POINT('',(0.,2.5,6.58));
#5476=CARTESIAN_POINT('',(0.,2.5,5.));
#5477=UNCERTAINTY_MEASURE_WITH_UNIT(LENGTH_MEASURE(0.001),#5503,
'DISTANCE_ACCURACY_VALUE',
'Maximum model space distance between geometric entities at asserted c
onnectivities');
#5478=UNCERTAINTY_MEASURE_WITH_UNIT(LENGTH_MEASURE(0.001),#5503,
'DISTANCE_ACCURACY_VALUE',
'Maximum model space distance between geometric entities at asserted c
onnectivities');
#5479=UNCERTAINTY_MEASURE_WITH_UNIT(LENGTH_MEASURE(0.001),#5503,
'DISTANCE_ACCURACY_VALUE',
'Maximum model space distance between geometric entities at asserted c
onnectivities');
#5480=UNCERTAINTY_MEASURE_WITH_UNIT(LENGTH_MEASURE(0.001),#5503,
'DISTANCE_ACCURACY_VALUE',
'Maximum model space distance between geometric entities at asserted c
onnectivities');
#5481=UNCERTAINTY_MEASURE_WITH_UNIT(LENGTH_MEASURE(0.001),#5503,
'DISTANCE_ACCURACY_VALUE',
'Maximum model space distance between geometric entities at asserted c
onnectivities');
#5482=UNCERTAINTY_MEASURE_WITH_UNIT(LENGTH_MEASURE(0.001),#5503,
'DISTANCE_ACCURACY_VALUE',
'Maximum model space distance between geometric entities at asserted c
onnectivities');
#5483=UNCERTAINTY_MEASURE_WITH_UNIT(LENGTH_MEASURE(0.001),#5503,
'DISTANCE_ACCURACY_VALUE',
'Maximum model space distance between geometric entities at asserted c
onnectivities');
#5484=UNCERTAINTY_MEASURE_WITH_UNIT(LENGTH_MEASURE(0.001),#5503,
'DISTANCE_ACCURACY_VALUE',
'Maximum model space distance between geometric entities at asserted c
onnectivities');
#5485=UNCERTAINTY_MEASURE_WITH_UNIT(LENGTH_MEASURE(0.001),#5503,
'DISTANCE_ACCURACY_VALUE',
'Maximum model space distance between geometric entities at asserted c
onnectivities');
#5486=UNCERTAINTY_MEASURE_WITH_UNIT(LENGTH_MEASURE(0.001),#5503,
'DISTANCE_ACCURACY_VALUE',
'Maximum model space distance between geometric entities at asserted c
onnectivities');
#5487=UNCERTAINTY_MEASURE_WITH_UNIT(LENGTH_MEASURE(0.001),#5503,
'DISTANCE_ACCURACY_VALUE',
'Maximum model space distance between geometric entities at asserted c
onnectivities');
#5488=UNCERTAINTY_MEASURE_WITH_UNIT(LENGTH_MEASURE(0.001),#5503,
'DISTANCE_ACCURACY_VALUE',
'Maximum model space distance between geometric entities at asserted c
onnectivities');
#5489=UNCERTAINTY_MEASURE_WITH_UNIT(LENGTH_MEASURE(0.001),#5503,
'DISTANCE_ACCURACY_VALUE',
'Maximum model space distance between geometric entities at asserted c
onnectivities');
#5490=(
GEOMETRIC_REPRESENTATION_CONTEXT(3)
GLOBAL_UNCERTAINTY_ASSIGNED_CONTEXT((#5477))
GLOBAL_UNIT_ASSIGNED_CONTEXT((#5503,#5505,#5506))
REPRESENTATION_CONTEXT('','3D')
);
#5491=(
GEOMETRIC_REPRESENTATION_CONTEXT(3)
GLOBAL_UNCERTAINTY_ASSIGNED_CONTEXT((#5478))
GLOBAL_UNIT_ASSIGNED_CONTEXT((#5503,#5505,#5506))
REPRESENTATION_CONTEXT('','3D')
);
#5492=(
GEOMETRIC_REPRESENTATION_CONTEXT(3)
GLOBAL_UNCERTAINTY_ASSIGNED_CONTEXT((#5479))
GLOBAL_UNIT_ASSIGNED_CONTEXT((#5503,#5505,#5506))
REPRESENTATION_CONTEXT('','3D')
);
#5493=(
GEOMETRIC_REPRESENTATION_CONTEXT(3)
GLOBAL_UNCERTAINTY_ASSIGNED_CONTEXT((#5480))
GLOBAL_UNIT_ASSIGNED_CONTEXT((#5503,#5505,#5506))
REPRESENTATION_CONTEXT('','3D')
);
#5494=(
GEOMETRIC_REPRESENTATION_CONTEXT(3)
GLOBAL_UNCERTAINTY_ASSIGNED_CONTEXT((#5481))
GLOBAL_UNIT_ASSIGNED_CONTEXT((#5503,#5505,#5506))
REPRESENTATION_CONTEXT('','3D')
);
#5495=(
GEOMETRIC_REPRESENTATION_CONTEXT(3)
GLOBAL_UNCERTAINTY_ASSIGNED_CONTEXT((#5482))
GLOBAL_UNIT_ASSIGNED_CONTEXT((#5503,#5505,#5506))
REPRESENTATION_CONTEXT('','3D')
);
#5496=(
GEOMETRIC_REPRESENTATION_CONTEXT(3)
GLOBAL_UNCERTAINTY_ASSIGNED_CONTEXT((#5483))
GLOBAL_UNIT_ASSIGNED_CONTEXT((#5503,#5505,#5506))
REPRESENTATION_CONTEXT('','3D')
);
#5497=(
GEOMETRIC_REPRESENTATION_CONTEXT(3)
GLOBAL_UNCERTAINTY_ASSIGNED_CONTEXT((#5484))
GLOBAL_UNIT_ASSIGNED_CONTEXT((#5503,#5505,#5506))
REPRESENTATION_CONTEXT('','3D')
);
#5498=(
GEOMETRIC_REPRESENTATION_CONTEXT(3)
GLOBAL_UNCERTAINTY_ASSIGNED_CONTEXT((#5485))
GLOBAL_UNIT_ASSIGNED_CONTEXT((#5503,#5505,#5506))
REPRESENTATION_CONTEXT('','3D')
);
#5499=(
GEOMETRIC_REPRESENTATION_CONTEXT(3)
GLOBAL_UNCERTAINTY_ASSIGNED_CONTEXT((#5486))
GLOBAL_UNIT_ASSIGNED_CONTEXT((#5503,#5505,#5506))
REPRESENTATION_CONTEXT('','3D')
);
#5500=(
GEOMETRIC_REPRESENTATION_CONTEXT(3)
GLOBAL_UNCERTAINTY_ASSIGNED_CONTEXT((#5487))
GLOBAL_UNIT_ASSIGNED_CONTEXT((#5503,#5505,#5506))
REPRESENTATION_CONTEXT('','3D')
);
#5501=(
GEOMETRIC_REPRESENTATION_CONTEXT(3)
GLOBAL_UNCERTAINTY_ASSIGNED_CONTEXT((#5488))
GLOBAL_UNIT_ASSIGNED_CONTEXT((#5503,#5505,#5506))
REPRESENTATION_CONTEXT('','3D')
);
#5502=(
GEOMETRIC_REPRESENTATION_CONTEXT(3)
GLOBAL_UNCERTAINTY_ASSIGNED_CONTEXT((#5489))
GLOBAL_UNIT_ASSIGNED_CONTEXT((#5503,#5505,#5506))
REPRESENTATION_CONTEXT('','3D')
);
#5503=(
LENGTH_UNIT()
NAMED_UNIT(*)
SI_UNIT(.CENTI.,.METRE.)
);
#5504=(
LENGTH_UNIT()
NAMED_UNIT(*)
SI_UNIT($,.METRE.)
);
#5505=(
NAMED_UNIT(*)
PLANE_ANGLE_UNIT()
SI_UNIT($,.RADIAN.)
);
#5506=(
NAMED_UNIT(*)
SI_UNIT($,.STERADIAN.)
SOLID_ANGLE_UNIT()
);
#5507=SHAPE_DEFINITION_REPRESENTATION(#5519,#5554);
#5508=SHAPE_DEFINITION_REPRESENTATION(#5520,#5555);
#5509=SHAPE_DEFINITION_REPRESENTATION(#5521,#5556);
#5510=SHAPE_DEFINITION_REPRESENTATION(#5522,#5557);
#5511=SHAPE_DEFINITION_REPRESENTATION(#5523,#5558);
#5512=SHAPE_DEFINITION_REPRESENTATION(#5524,#5559);
#5513=SHAPE_DEFINITION_REPRESENTATION(#5525,#5560);
#5514=SHAPE_DEFINITION_REPRESENTATION(#5526,#5561);
#5515=SHAPE_DEFINITION_REPRESENTATION(#5527,#5562);
#5516=SHAPE_DEFINITION_REPRESENTATION(#5531,#5563);
#5517=SHAPE_DEFINITION_REPRESENTATION(#5532,#5564);
#5518=SHAPE_DEFINITION_REPRESENTATION(#5533,#5565);
#5519=PRODUCT_DEFINITION_SHAPE('',$,#5567);
#5520=PRODUCT_DEFINITION_SHAPE('',$,#5568);
#5521=PRODUCT_DEFINITION_SHAPE('',$,#5569);
#5522=PRODUCT_DEFINITION_SHAPE('',$,#5570);
#5523=PRODUCT_DEFINITION_SHAPE('',$,#5571);
#5524=PRODUCT_DEFINITION_SHAPE('',$,#5572);
#5525=PRODUCT_DEFINITION_SHAPE('',$,#5573);
#5526=PRODUCT_DEFINITION_SHAPE('',$,#5574);
#5527=PRODUCT_DEFINITION_SHAPE('',$,#5575);
#5528=PRODUCT_DEFINITION_SHAPE($,$,#92);
#5529=PRODUCT_DEFINITION_SHAPE($,$,#93);
#5530=PRODUCT_DEFINITION_SHAPE($,$,#94);
#5531=PRODUCT_DEFINITION_SHAPE('',$,#5576);
#5532=PRODUCT_DEFINITION_SHAPE('',$,#5577);
#5533=PRODUCT_DEFINITION_SHAPE('',$,#5578);
#5534=PRODUCT_DEFINITION_SHAPE($,$,#95);
#5535=PRODUCT_DEFINITION_SHAPE($,$,#96);
#5536=PRODUCT_DEFINITION_SHAPE($,$,#97);
#5537=PRODUCT_DEFINITION_SHAPE($,$,#98);
#5538=PRODUCT_DEFINITION_SHAPE($,$,#99);
#5539=PRODUCT_DEFINITION_SHAPE($,$,#100);
#5540=PRODUCT_DEFINITION_SHAPE($,$,#101);
#5541=PRODUCT_DEFINITION_SHAPE($,$,#102);
#5542=PRODUCT_DEFINITION_SHAPE($,$,#103);
#5543=PRODUCT_DEFINITION_SHAPE($,$,#104);
#5544=PRODUCT_DEFINITION_SHAPE($,$,#105);
#5545=PRODUCT_DEFINITION_SHAPE($,$,#106);
#5546=PRODUCT_DEFINITION_SHAPE($,$,#107);
#5547=PRODUCT_DEFINITION_SHAPE($,$,#108);
#5548=PRODUCT_DEFINITION_SHAPE($,$,#109);
#5549=PRODUCT_DEFINITION_SHAPE($,$,#110);
#5550=PRODUCT_DEFINITION_SHAPE($,$,#111);
#5551=PRODUCT_DEFINITION_SHAPE($,$,#112);
#5552=PRODUCT_DEFINITION_SHAPE($,$,#113);
#5553=PRODUCT_DEFINITION_SHAPE($,$,#114);
#5554=SHAPE_REPRESENTATION('',(#3327,#3598,#3599,#3600,#3601,#3602,#3603,
#3604,#3605,#3606,#3607,#3608,#3609,#3610,#3611,#3612,#3613,#3614,#3615,
#3616,#3617),#5490);
#5555=SHAPE_REPRESENTATION('',(#3328),#5491);
#5556=SHAPE_REPRESENTATION('',(#3344),#5492);
#5557=SHAPE_REPRESENTATION('',(#3411),#5493);
#5558=SHAPE_REPRESENTATION('',(#3442),#5494);
#5559=SHAPE_REPRESENTATION('',(#3463,#3521,#3522,#3523),#5495);
#5560=SHAPE_REPRESENTATION('',(#3464),#5496);
#5561=SHAPE_REPRESENTATION('',(#3481),#5497);
#5562=SHAPE_REPRESENTATION('',(#3496),#5498);
#5563=SHAPE_REPRESENTATION('',(#3524),#5499);
#5564=SHAPE_REPRESENTATION('',(#3548),#5500);
#5565=SHAPE_REPRESENTATION('',(#3577),#5501);
#5566=PRODUCT_DEFINITION_CONTEXT('part definition',#5604,'design');
#5567=PRODUCT_DEFINITION('PAT-065',
'PAT-065',#5579,#5566);
#5568=PRODUCT_DEFINITION('Corner foot bracket',
'Corner foot bracket',#5580,#5566);
#5569=PRODUCT_DEFINITION('Slotted Extrusion - 20 x 20 x 100 mm',
'Slotted Extrusion - 20 x 20 x 100 mm',#5581,#5566);
#5570=PRODUCT_DEFINITION('Corner Gusset - 20 mm Extrusion',
'Corner Gusset - 20 mm Extrusion',#5582,#5566);
#5571=PRODUCT_DEFINITION('Low-profile M5x8 gusset screw',
'Low-profile M5x8 gusset screw',#5583,#5566);
#5572=PRODUCT_DEFINITION('Levelling Foot - 40 mm Pad, M8 Stud',
'Levelling Foot - 40 mm Pad, M8 Stud',#5584,#5566);
#5573=PRODUCT_DEFINITION('Rubber base','Rubber base',#5585,
#5566);
#5574=PRODUCT_DEFINITION('Steel pad','Steel pad',#5586,
#5566);
#5575=PRODUCT_DEFINITION('Stud','Stud',#5587,#5566);
#5576=PRODUCT_DEFINITION('Hex Nut - M8','Hex Nut - M8',#5588,
#5566);
#5577=PRODUCT_DEFINITION('Slot Nut - M5 for 20 mm Extrusion',
'Slot Nut - M5 for 20 mm Extrusion',#5589,#5566);
#5578=PRODUCT_DEFINITION('M5x14 Cap Screw','M5x14 Cap Screw',
#5590,#5566);
#5579=PRODUCT_DEFINITION_FORMATION('',$,#5606);
#5580=PRODUCT_DEFINITION_FORMATION('',$,#5607);
#5581=PRODUCT_DEFINITION_FORMATION('',$,#5608);
#5582=PRODUCT_DEFINITION_FORMATION('',$,#5609);
#5583=PRODUCT_DEFINITION_FORMATION('',$,#5610);
#5584=PRODUCT_DEFINITION_FORMATION('',$,#5611);
#5585=PRODUCT_DEFINITION_FORMATION('',$,#5612);
#5586=PRODUCT_DEFINITION_FORMATION('',$,#5613);
#5587=PRODUCT_DEFINITION_FORMATION('',$,#5614);
#5588=PRODUCT_DEFINITION_FORMATION('',$,#5615);
#5589=PRODUCT_DEFINITION_FORMATION('',$,#5616);
#5590=PRODUCT_DEFINITION_FORMATION('',$,#5617);
#5591=PRODUCT_RELATED_PRODUCT_CATEGORY(
'PAT-065','PAT-065',(#5606));
#5592=PRODUCT_RELATED_PRODUCT_CATEGORY('Corner foot bracket',
'Corner foot bracket',(#5607));
#5593=PRODUCT_RELATED_PRODUCT_CATEGORY(
'Slotted Extrusion - 20 x 20 x 100 mm',
'Slotted Extrusion - 20 x 20 x 100 mm',(#5608));
#5594=PRODUCT_RELATED_PRODUCT_CATEGORY(
'Corner Gusset - 20 mm Extrusion','Corner Gusset - 20 mm Extrusion',(#5609));
#5595=PRODUCT_RELATED_PRODUCT_CATEGORY('Low-profile M5x8 gusset screw',
'Low-profile M5x8 gusset screw',(#5610));
#5596=PRODUCT_RELATED_PRODUCT_CATEGORY(
'Levelling Foot - 40 mm Pad, M8 Stud',
'Levelling Foot - 40 mm Pad, M8 Stud',(#5611));
#5597=PRODUCT_RELATED_PRODUCT_CATEGORY('Rubber base','Rubber base',(#5612));
#5598=PRODUCT_RELATED_PRODUCT_CATEGORY('Steel pad','Steel pad',(#5613));
#5599=PRODUCT_RELATED_PRODUCT_CATEGORY('Stud','Stud',(#5614));
#5600=PRODUCT_RELATED_PRODUCT_CATEGORY('Hex Nut - M8','Hex Nut - M8',(#5615));
#5601=PRODUCT_RELATED_PRODUCT_CATEGORY(
'Slot Nut - M5 for 20 mm Extrusion','Slot Nut - M5 for 20 mm Extrusion',
(#5616));
#5602=PRODUCT_RELATED_PRODUCT_CATEGORY('M5x14 Cap Screw',
'M5x14 Cap Screw',(#5617));
#5603=APPLICATION_PROTOCOL_DEFINITION('international standard',
'automotive_design',2009,#5604);
#5604=APPLICATION_CONTEXT(
'Core Data for Automotive Mechanical Design Process');
#5605=PRODUCT_CONTEXT('part definition',#5604,'mechanical');
#5606=PRODUCT('PAT-065',
'PAT-065','PAT-065',(#5605));
#5607=PRODUCT('Corner foot bracket','Corner foot bracket',
'Corner foot bracket',(#5605));
#5608=PRODUCT('Slotted Extrusion - 20 x 20 x 100 mm',
'Slotted Extrusion - 20 x 20 x 100 mm',
'Slotted Extrusion - 20 x 20 x 100 mm',(#5605));
#5609=PRODUCT('Corner Gusset - 20 mm Extrusion',
'Corner Gusset - 20 mm Extrusion','Corner Gusset - 20 mm Extrusion',(#5605));
#5610=PRODUCT('Low-profile M5x8 gusset screw','Low-profile M5x8 gusset screw',
'Low-profile M5x8 gusset screw',(#5605));
#5611=PRODUCT('Levelling Foot - 40 mm Pad, M8 Stud',
'Levelling Foot - 40 mm Pad, M8 Stud',
'Levelling Foot - 40 mm Pad, M8 Stud',(#5605));
#5612=PRODUCT('Rubber base','Rubber base','Rubber base',(#5605));
#5613=PRODUCT('Steel pad','Steel pad','Steel pad',(#5605));
#5614=PRODUCT('Stud','Stud','Stud',(#5605));
#5615=PRODUCT('Hex Nut - M8','Hex Nut - M8','Hex Nut - M8',
(#5605));
#5616=PRODUCT('Slot Nut - M5 for 20 mm Extrusion',
'Slot Nut - M5 for 20 mm Extrusion','Slot Nut - M5 for 20 mm Extrusion',
(#5605));
#5617=PRODUCT('M5x14 Cap Screw','M5x14 Cap Screw',
'M5x14 Cap Screw',(#5605));
#5618=PRESENTATION_STYLE_ASSIGNMENT((#5625));
#5619=PRESENTATION_STYLE_ASSIGNMENT((#5626));
#5620=PRESENTATION_STYLE_ASSIGNMENT((#5627));
#5621=PRESENTATION_STYLE_ASSIGNMENT((#5628));
#5622=PRESENTATION_STYLE_ASSIGNMENT((#5629));
#5623=PRESENTATION_STYLE_ASSIGNMENT((#5630));
#5624=PRESENTATION_STYLE_ASSIGNMENT((#5631));
#5625=SURFACE_STYLE_USAGE(.BOTH.,#5632);
#5626=SURFACE_STYLE_USAGE(.BOTH.,#5633);
#5627=SURFACE_STYLE_USAGE(.BOTH.,#5634);
#5628=SURFACE_STYLE_USAGE(.BOTH.,#5635);
#5629=SURFACE_STYLE_USAGE(.BOTH.,#5636);
#5630=SURFACE_STYLE_USAGE(.BOTH.,#5637);
#5631=SURFACE_STYLE_USAGE(.BOTH.,#5638);
#5632=SURFACE_SIDE_STYLE('',(#5639));
#5633=SURFACE_SIDE_STYLE('',(#5640));
#5634=SURFACE_SIDE_STYLE('',(#5641));
#5635=SURFACE_SIDE_STYLE('',(#5642));
#5636=SURFACE_SIDE_STYLE('',(#5643));
#5637=SURFACE_SIDE_STYLE('',(#5644));
#5638=SURFACE_SIDE_STYLE('',(#5645));
#5639=SURFACE_STYLE_FILL_AREA(#5646);
#5640=SURFACE_STYLE_FILL_AREA(#5647);
#5641=SURFACE_STYLE_FILL_AREA(#5648);
#5642=SURFACE_STYLE_FILL_AREA(#5649);
#5643=SURFACE_STYLE_FILL_AREA(#5650);
#5644=SURFACE_STYLE_FILL_AREA(#5651);
#5645=SURFACE_STYLE_FILL_AREA(#5652);
#5646=FILL_AREA_STYLE('Steel - Satin',(#5653));
#5647=FILL_AREA_STYLE('CAD Library Painted - Deep blue',(#5654));
#5648=FILL_AREA_STYLE('CAD Library Painted - Steel gray',(#5655));
#5649=FILL_AREA_STYLE('CAD Library Painted - Light blue',(#5656));
#5650=FILL_AREA_STYLE('CAD Library Painted - Graphite',(#5657));
#5651=FILL_AREA_STYLE('CAD Library Painted - Off white',(#5658));
#5652=FILL_AREA_STYLE('CAD Library Painted - Engineering blue',(#5659));
#5653=FILL_AREA_STYLE_COLOUR('Steel - Satin',#5660);
#5654=FILL_AREA_STYLE_COLOUR('CAD Library Painted - Deep blue',#5661);
#5655=FILL_AREA_STYLE_COLOUR('CAD Library Painted - Steel gray',#5662);
#5656=FILL_AREA_STYLE_COLOUR('CAD Library Painted - Light blue',#5663);
#5657=FILL_AREA_STYLE_COLOUR('CAD Library Painted - Graphite',#5664);
#5658=FILL_AREA_STYLE_COLOUR('CAD Library Painted - Off white',#5665);
#5659=FILL_AREA_STYLE_COLOUR('CAD Library Painted - Engineering blue',#5666);
#5660=COLOUR_RGB('Steel - Satin',0.627450980392157,0.627450980392157,0.627450980392157);
#5661=COLOUR_RGB('CAD Library Painted - Deep blue',0.0784313725490196,0.203921568627451,
0.349019607843137);
#5662=COLOUR_RGB('CAD Library Painted - Steel gray',0.592156862745098,0.631372549019608,
0.67843137254902);
#5663=COLOUR_RGB('CAD Library Painted - Light blue',0.286274509803922,0.552941176470588,
0.780392156862745);
#5664=COLOUR_RGB('CAD Library Painted - Graphite',0.0980392156862745,0.109803921568627,
0.125490196078431);
#5665=COLOUR_RGB('CAD Library Painted - Off white',0.909803921568627,0.901960784313726,
0.858823529411765);
#5666=COLOUR_RGB('CAD Library Painted - Engineering blue',0.12156862745098,
0.356862745098039,0.6);
#5667=COLOUR_RGB('Dark Blue',0.08,0.2,0.34);
#5668=FILL_AREA_STYLE_COLOUR('',#5667);
#5669=FILL_AREA_STYLE('',(#5668));
#5670=SURFACE_STYLE_FILL_AREA(#5669);
#5671=SURFACE_SIDE_STYLE('',(#5670));
#5672=SURFACE_STYLE_USAGE(.BOTH.,#5671);
#5673=PRESENTATION_STYLE_ASSIGNMENT((#5672));
#5674=COLOUR_RGB('Light Blue',0.38,0.62,0.78);
#5675=FILL_AREA_STYLE_COLOUR('',#5674);
#5676=FILL_AREA_STYLE('',(#5675));
#5677=SURFACE_STYLE_FILL_AREA(#5676);
#5678=SURFACE_SIDE_STYLE('',(#5677));
#5679=SURFACE_STYLE_USAGE(.BOTH.,#5678);
#5680=PRESENTATION_STYLE_ASSIGNMENT((#5679));
#5681=COLOUR_RGB('Sky Blue',0.24,0.69,0.87);
#5682=FILL_AREA_STYLE_COLOUR('',#5681);
#5683=FILL_AREA_STYLE('',(#5682));
#5684=SURFACE_STYLE_FILL_AREA(#5683);
#5685=SURFACE_SIDE_STYLE('',(#5684));
#5686=SURFACE_STYLE_USAGE(.BOTH.,#5685);
#5687=PRESENTATION_STYLE_ASSIGNMENT((#5686));
#5688=COLOUR_RGB('Grey',0.48,0.52,0.57);
#5689=FILL_AREA_STYLE_COLOUR('',#5688);
#5690=FILL_AREA_STYLE('',(#5689));
#5691=SURFACE_STYLE_FILL_AREA(#5690);
#5692=SURFACE_SIDE_STYLE('',(#5691));
#5693=SURFACE_STYLE_USAGE(.BOTH.,#5692);
#5694=PRESENTATION_STYLE_ASSIGNMENT((#5693));
#5695=COLOUR_RGB('Black',0.12,0.14,0.17);
#5696=FILL_AREA_STYLE_COLOUR('',#5695);
#5697=FILL_AREA_STYLE('',(#5696));
#5698=SURFACE_STYLE_FILL_AREA(#5697);
#5699=SURFACE_SIDE_STYLE('',(#5698));
#5700=SURFACE_STYLE_USAGE(.BOTH.,#5699);
#5701=PRESENTATION_STYLE_ASSIGNMENT((#5700));
#5702=COLOUR_RGB('Off White',0.89,0.88,0.83);
#5703=FILL_AREA_STYLE_COLOUR('',#5702);
#5704=FILL_AREA_STYLE('',(#5703));
#5705=SURFACE_STYLE_FILL_AREA(#5704);
#5706=SURFACE_SIDE_STYLE('',(#5705));
#5707=SURFACE_STYLE_USAGE(.BOTH.,#5706);
#5708=PRESENTATION_STYLE_ASSIGNMENT((#5707));
ENDSEC;
END-ISO-10303-21;
